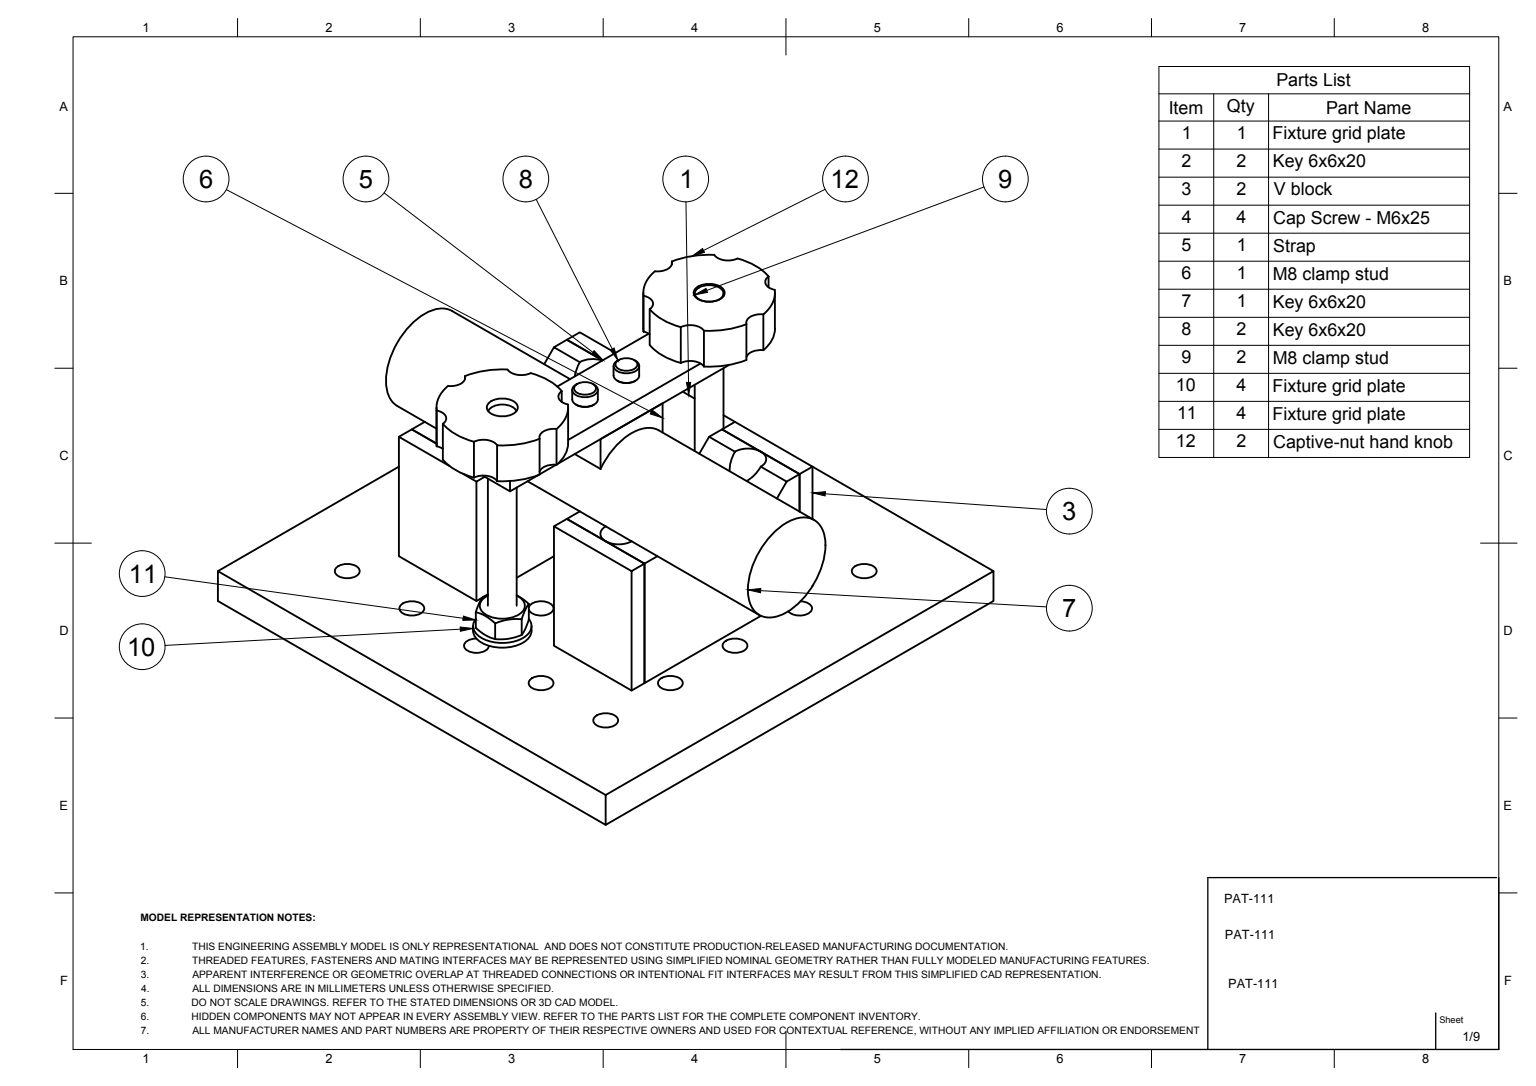
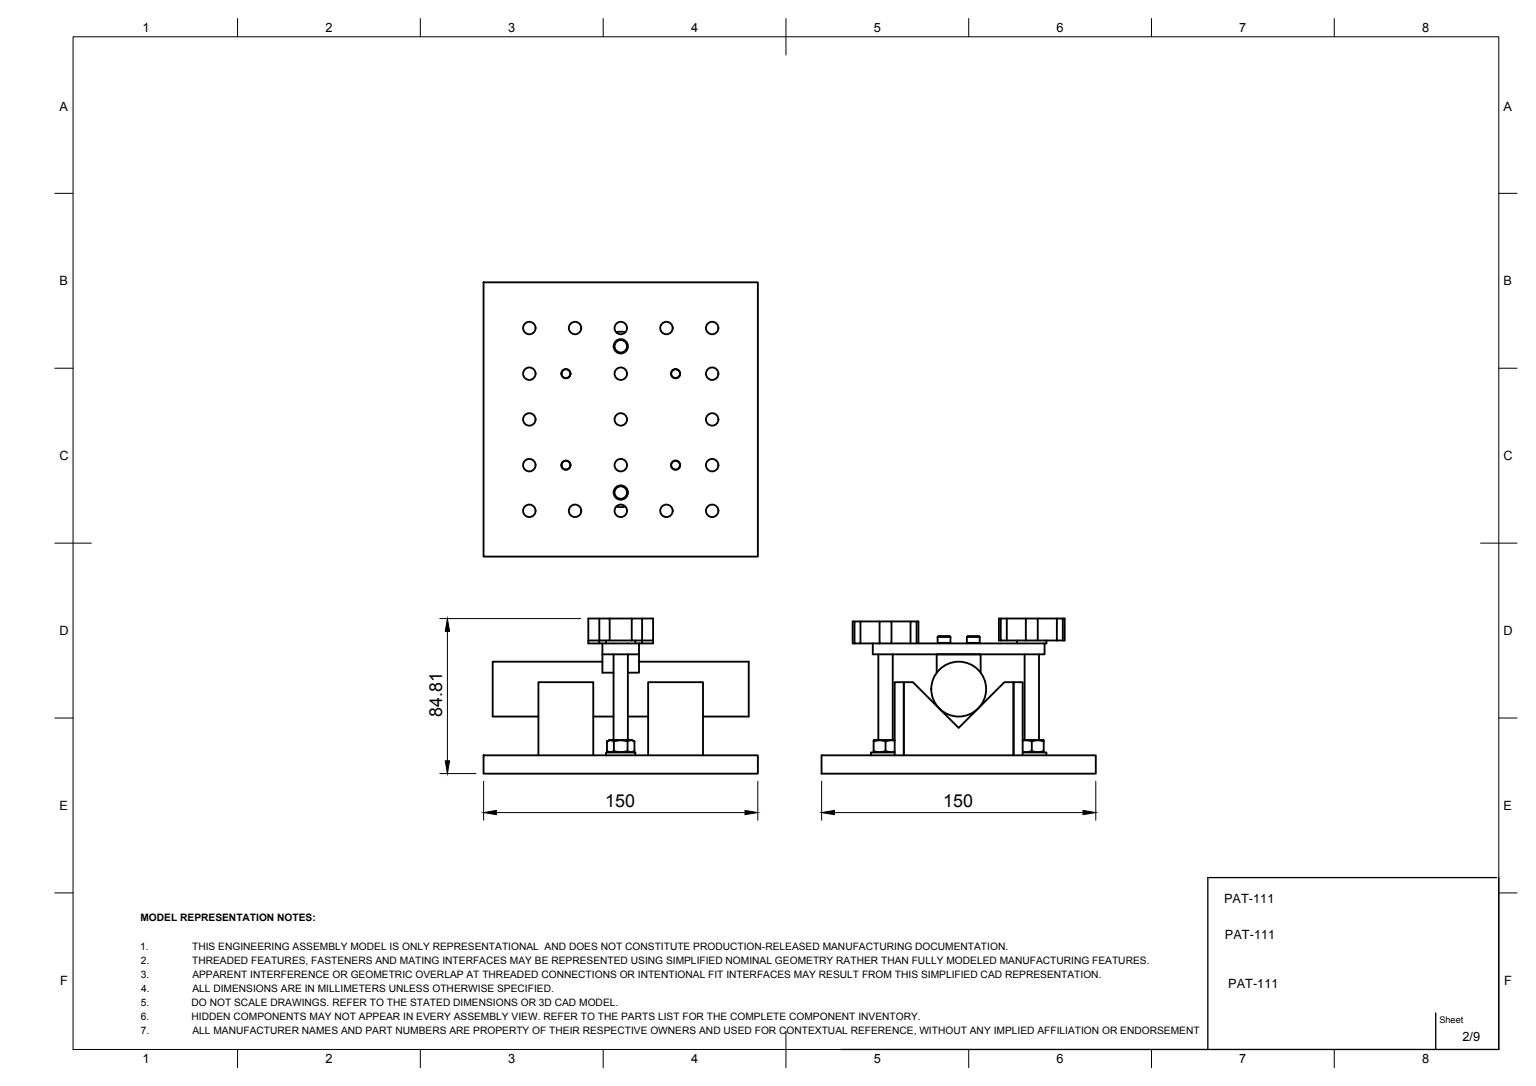
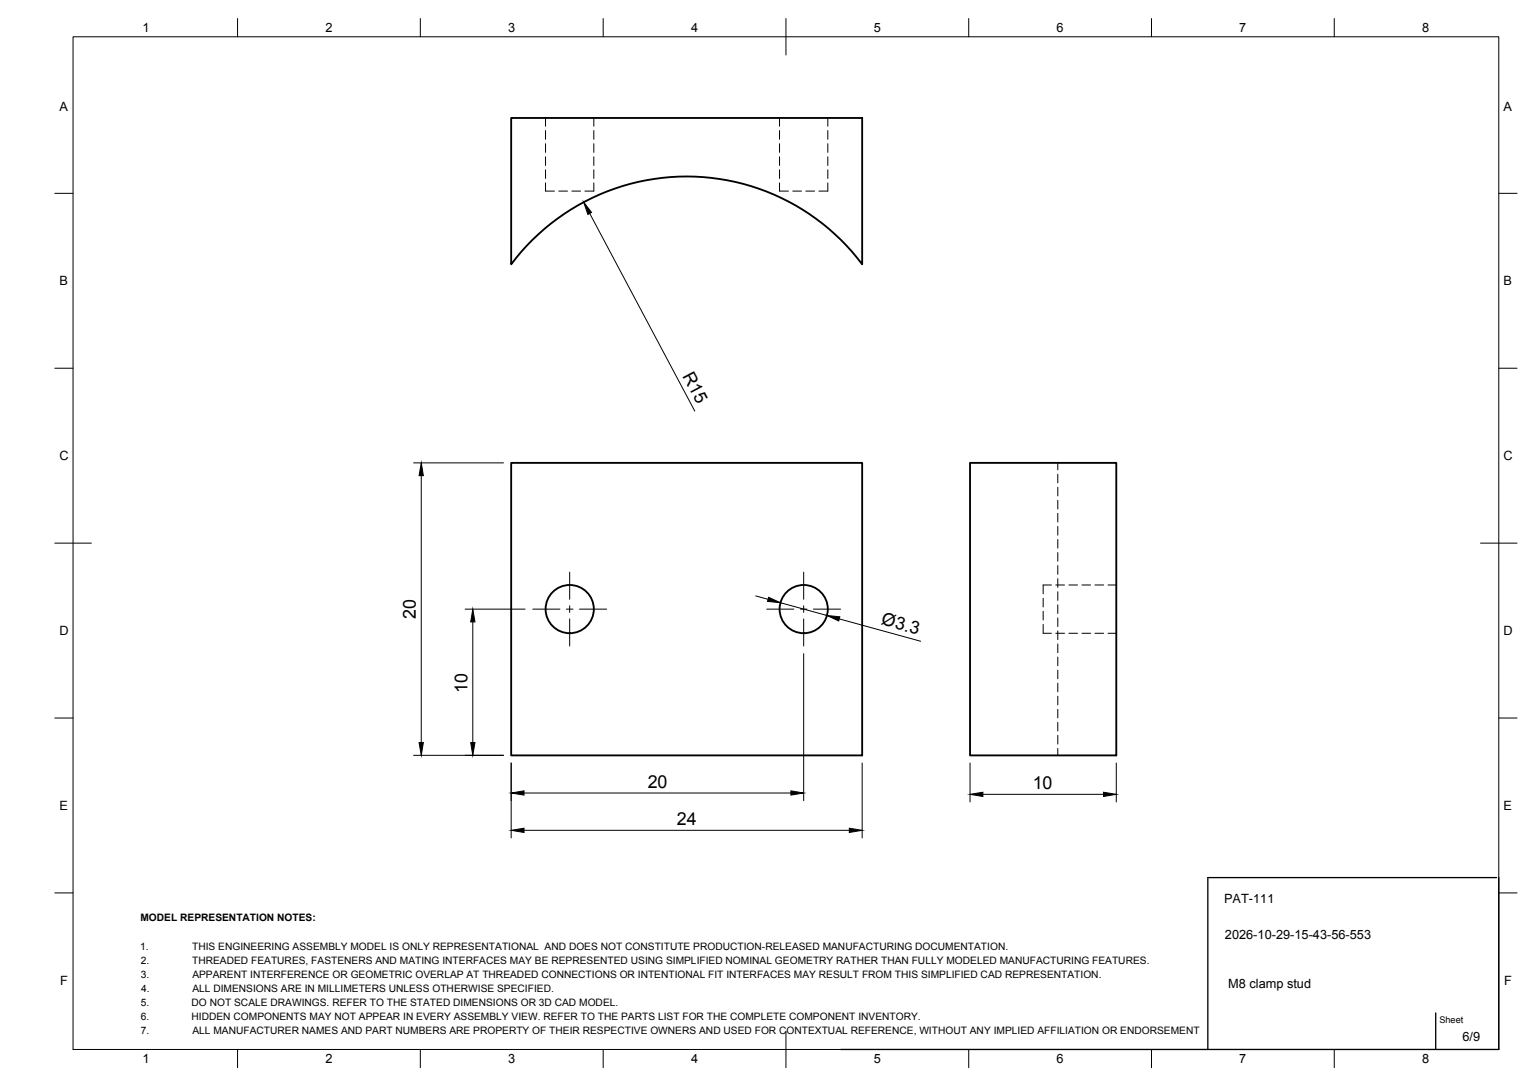
ISO-10303-21;
HEADER;
/* Generated by software containing ST-Developer
 * from STEP Tools, Inc. (www.steptools.com) 
 */

FILE_DESCRIPTION(
/* description */ ('Grid plate located blocks and clamp'),
/* implementation_level */ '2;1');

FILE_NAME(
/* name */ 'PAT-111',
/* time_stamp */ '2026-10-29T15:43:47-07:00',
/* author */ (''),
/* organization */ (''),
/* preprocessor_version */ 'ST-DEVELOPER v20.2',
/* originating_system */ 'Autodesk Translation Framework v15.17.0.0',
/* authorisation */ '');

FILE_SCHEMA (('AUTOMOTIVE_DESIGN { 1 0 10303 214 3 1 1 }'));
ENDSEC;

DATA;
#10=MECHANICAL_DESIGN_GEOMETRIC_PRESENTATION_REPRESENTATION('',(#166,#167,
#168,#169,#170,#171,#172,#173,#174,#175,#176,#177,#178,#179),#5702);
#11=ITEM_DEFINED_TRANSFORMATION($,$,#3411,#3737);
#12=ITEM_DEFINED_TRANSFORMATION($,$,#3688,#3738);
#13=ITEM_DEFINED_TRANSFORMATION($,$,#3503,#3739);
#14=ITEM_DEFINED_TRANSFORMATION($,$,#3514,#3740);
#15=ITEM_DEFINED_TRANSFORMATION($,$,#3565,#3741);
#16=ITEM_DEFINED_TRANSFORMATION($,$,#3565,#3742);
#17=ITEM_DEFINED_TRANSFORMATION($,$,#3503,#3743);
#18=ITEM_DEFINED_TRANSFORMATION($,$,#3514,#3744);
#19=ITEM_DEFINED_TRANSFORMATION($,$,#3565,#3745);
#20=ITEM_DEFINED_TRANSFORMATION($,$,#3565,#3746);
#21=ITEM_DEFINED_TRANSFORMATION($,$,#3591,#3747);
#22=ITEM_DEFINED_TRANSFORMATION($,$,#3610,#3748);
#23=ITEM_DEFINED_TRANSFORMATION($,$,#3627,#3749);
#24=ITEM_DEFINED_TRANSFORMATION($,$,#3633,#3750);
#25=ITEM_DEFINED_TRANSFORMATION($,$,#3633,#3751);
#26=ITEM_DEFINED_TRANSFORMATION($,$,#3657,#3752);
#27=ITEM_DEFINED_TRANSFORMATION($,$,#3663,#3753);
#28=ITEM_DEFINED_TRANSFORMATION($,$,#3663,#3754);
#29=ITEM_DEFINED_TRANSFORMATION($,$,#3672,#3755);
#30=ITEM_DEFINED_TRANSFORMATION($,$,#3672,#3756);
#31=ITEM_DEFINED_TRANSFORMATION($,$,#3657,#3757);
#32=ITEM_DEFINED_TRANSFORMATION($,$,#3663,#3758);
#33=ITEM_DEFINED_TRANSFORMATION($,$,#3663,#3759);
#34=ITEM_DEFINED_TRANSFORMATION($,$,#3672,#3760);
#35=ITEM_DEFINED_TRANSFORMATION($,$,#3672,#3761);
#36=ITEM_DEFINED_TRANSFORMATION($,$,#3688,#3762);
#37=(
REPRESENTATION_RELATIONSHIP($,$,#5760,#5759)
REPRESENTATION_RELATIONSHIP_WITH_TRANSFORMATION(#11)
SHAPE_REPRESENTATION_RELATIONSHIP()
);
#38=(
REPRESENTATION_RELATIONSHIP($,$,#5771,#5759)
REPRESENTATION_RELATIONSHIP_WITH_TRANSFORMATION(#12)
SHAPE_REPRESENTATION_RELATIONSHIP()
);
#39=(
REPRESENTATION_RELATIONSHIP($,$,#5761,#5759)
REPRESENTATION_RELATIONSHIP_WITH_TRANSFORMATION(#13)
SHAPE_REPRESENTATION_RELATIONSHIP()
);
#40=(
REPRESENTATION_RELATIONSHIP($,$,#5762,#5759)
REPRESENTATION_RELATIONSHIP_WITH_TRANSFORMATION(#14)
SHAPE_REPRESENTATION_RELATIONSHIP()
);
#41=(
REPRESENTATION_RELATIONSHIP($,$,#5763,#5759)
REPRESENTATION_RELATIONSHIP_WITH_TRANSFORMATION(#15)
SHAPE_REPRESENTATION_RELATIONSHIP()
);
#42=(
REPRESENTATION_RELATIONSHIP($,$,#5763,#5759)
REPRESENTATION_RELATIONSHIP_WITH_TRANSFORMATION(#16)
SHAPE_REPRESENTATION_RELATIONSHIP()
);
#43=(
REPRESENTATION_RELATIONSHIP($,$,#5761,#5759)
REPRESENTATION_RELATIONSHIP_WITH_TRANSFORMATION(#17)
SHAPE_REPRESENTATION_RELATIONSHIP()
);
#44=(
REPRESENTATION_RELATIONSHIP($,$,#5762,#5759)
REPRESENTATION_RELATIONSHIP_WITH_TRANSFORMATION(#18)
SHAPE_REPRESENTATION_RELATIONSHIP()
);
#45=(
REPRESENTATION_RELATIONSHIP($,$,#5763,#5759)
REPRESENTATION_RELATIONSHIP_WITH_TRANSFORMATION(#19)
SHAPE_REPRESENTATION_RELATIONSHIP()
);
#46=(
REPRESENTATION_RELATIONSHIP($,$,#5763,#5759)
REPRESENTATION_RELATIONSHIP_WITH_TRANSFORMATION(#20)
SHAPE_REPRESENTATION_RELATIONSHIP()
);
#47=(
REPRESENTATION_RELATIONSHIP($,$,#5764,#5759)
REPRESENTATION_RELATIONSHIP_WITH_TRANSFORMATION(#21)
SHAPE_REPRESENTATION_RELATIONSHIP()
);
#48=(
REPRESENTATION_RELATIONSHIP($,$,#5765,#5759)
REPRESENTATION_RELATIONSHIP_WITH_TRANSFORMATION(#22)
SHAPE_REPRESENTATION_RELATIONSHIP()
);
#49=(
REPRESENTATION_RELATIONSHIP($,$,#5766,#5759)
REPRESENTATION_RELATIONSHIP_WITH_TRANSFORMATION(#23)
SHAPE_REPRESENTATION_RELATIONSHIP()
);
#50=(
REPRESENTATION_RELATIONSHIP($,$,#5767,#5759)
REPRESENTATION_RELATIONSHIP_WITH_TRANSFORMATION(#24)
SHAPE_REPRESENTATION_RELATIONSHIP()
);
#51=(
REPRESENTATION_RELATIONSHIP($,$,#5767,#5759)
REPRESENTATION_RELATIONSHIP_WITH_TRANSFORMATION(#25)
SHAPE_REPRESENTATION_RELATIONSHIP()
);
#52=(
REPRESENTATION_RELATIONSHIP($,$,#5768,#5759)
REPRESENTATION_RELATIONSHIP_WITH_TRANSFORMATION(#26)
SHAPE_REPRESENTATION_RELATIONSHIP()
);
#53=(
REPRESENTATION_RELATIONSHIP($,$,#5769,#5759)
REPRESENTATION_RELATIONSHIP_WITH_TRANSFORMATION(#27)
SHAPE_REPRESENTATION_RELATIONSHIP()
);
#54=(
REPRESENTATION_RELATIONSHIP($,$,#5769,#5759)
REPRESENTATION_RELATIONSHIP_WITH_TRANSFORMATION(#28)
SHAPE_REPRESENTATION_RELATIONSHIP()
);
#55=(
REPRESENTATION_RELATIONSHIP($,$,#5770,#5759)
REPRESENTATION_RELATIONSHIP_WITH_TRANSFORMATION(#29)
SHAPE_REPRESENTATION_RELATIONSHIP()
);
#56=(
REPRESENTATION_RELATIONSHIP($,$,#5770,#5759)
REPRESENTATION_RELATIONSHIP_WITH_TRANSFORMATION(#30)
SHAPE_REPRESENTATION_RELATIONSHIP()
);
#57=(
REPRESENTATION_RELATIONSHIP($,$,#5768,#5759)
REPRESENTATION_RELATIONSHIP_WITH_TRANSFORMATION(#31)
SHAPE_REPRESENTATION_RELATIONSHIP()
);
#58=(
REPRESENTATION_RELATIONSHIP($,$,#5769,#5759)
REPRESENTATION_RELATIONSHIP_WITH_TRANSFORMATION(#32)
SHAPE_REPRESENTATION_RELATIONSHIP()
);
#59=(
REPRESENTATION_RELATIONSHIP($,$,#5769,#5759)
REPRESENTATION_RELATIONSHIP_WITH_TRANSFORMATION(#33)
SHAPE_REPRESENTATION_RELATIONSHIP()
);
#60=(
REPRESENTATION_RELATIONSHIP($,$,#5770,#5759)
REPRESENTATION_RELATIONSHIP_WITH_TRANSFORMATION(#34)
SHAPE_REPRESENTATION_RELATIONSHIP()
);
#61=(
REPRESENTATION_RELATIONSHIP($,$,#5770,#5759)
REPRESENTATION_RELATIONSHIP_WITH_TRANSFORMATION(#35)
SHAPE_REPRESENTATION_RELATIONSHIP()
);
#62=(
REPRESENTATION_RELATIONSHIP($,$,#5771,#5759)
REPRESENTATION_RELATIONSHIP_WITH_TRANSFORMATION(#36)
SHAPE_REPRESENTATION_RELATIONSHIP()
);
#63=CONTEXT_DEPENDENT_SHAPE_REPRESENTATION(#37,#5733);
#64=CONTEXT_DEPENDENT_SHAPE_REPRESENTATION(#38,#5734);
#65=CONTEXT_DEPENDENT_SHAPE_REPRESENTATION(#39,#5735);
#66=CONTEXT_DEPENDENT_SHAPE_REPRESENTATION(#40,#5736);
#67=CONTEXT_DEPENDENT_SHAPE_REPRESENTATION(#41,#5737);
#68=CONTEXT_DEPENDENT_SHAPE_REPRESENTATION(#42,#5738);
#69=CONTEXT_DEPENDENT_SHAPE_REPRESENTATION(#43,#5739);
#70=CONTEXT_DEPENDENT_SHAPE_REPRESENTATION(#44,#5740);
#71=CONTEXT_DEPENDENT_SHAPE_REPRESENTATION(#45,#5741);
#72=CONTEXT_DEPENDENT_SHAPE_REPRESENTATION(#46,#5742);
#73=CONTEXT_DEPENDENT_SHAPE_REPRESENTATION(#47,#5743);
#74=CONTEXT_DEPENDENT_SHAPE_REPRESENTATION(#48,#5744);
#75=CONTEXT_DEPENDENT_SHAPE_REPRESENTATION(#49,#5745);
#76=CONTEXT_DEPENDENT_SHAPE_REPRESENTATION(#50,#5746);
#77=CONTEXT_DEPENDENT_SHAPE_REPRESENTATION(#51,#5747);
#78=CONTEXT_DEPENDENT_SHAPE_REPRESENTATION(#52,#5748);
#79=CONTEXT_DEPENDENT_SHAPE_REPRESENTATION(#53,#5749);
#80=CONTEXT_DEPENDENT_SHAPE_REPRESENTATION(#54,#5750);
#81=CONTEXT_DEPENDENT_SHAPE_REPRESENTATION(#55,#5751);
#82=CONTEXT_DEPENDENT_SHAPE_REPRESENTATION(#56,#5752);
#83=CONTEXT_DEPENDENT_SHAPE_REPRESENTATION(#57,#5753);
#84=CONTEXT_DEPENDENT_SHAPE_REPRESENTATION(#58,#5754);
#85=CONTEXT_DEPENDENT_SHAPE_REPRESENTATION(#59,#5755);
#86=CONTEXT_DEPENDENT_SHAPE_REPRESENTATION(#60,#5756);
#87=CONTEXT_DEPENDENT_SHAPE_REPRESENTATION(#61,#5757);
#88=CONTEXT_DEPENDENT_SHAPE_REPRESENTATION(#62,#5758);
#89=NEXT_ASSEMBLY_USAGE_OCCURRENCE('Fixture grid plate:1',
'Fixture grid plate:1','Fixture grid plate:1',#5773,#5774,
'Fixture grid plate:1');
#90=NEXT_ASSEMBLY_USAGE_OCCURRENCE('Captive-nut hand knob:1',
'Captive-nut hand knob:1','Captive-nut hand knob:1',#5773,#5785,
'Captive-nut hand knob:1');
#91=NEXT_ASSEMBLY_USAGE_OCCURRENCE('Key 6x6x20:1','Key 6x6x20:1',
'Key 6x6x20:1',#5773,#5775,'Key 6x6x20:1');
#92=NEXT_ASSEMBLY_USAGE_OCCURRENCE('V block:1','V block:1','V block:1',
#5773,#5776,'V block:1');
#93=NEXT_ASSEMBLY_USAGE_OCCURRENCE('Cap Screw - M6x25:1',
'Cap Screw - M6x25:1','Cap Screw - M6x25:1',#5773,#5777,
'Cap Screw - M6x25:1');
#94=NEXT_ASSEMBLY_USAGE_OCCURRENCE('Cap Screw - M6x25:2',
'Cap Screw - M6x25:2','Cap Screw - M6x25:2',#5773,#5777,
'Cap Screw - M6x25:2');
#95=NEXT_ASSEMBLY_USAGE_OCCURRENCE('Key 6x6x20:2','Key 6x6x20:2',
'Key 6x6x20:2',#5773,#5775,'Key 6x6x20:2');
#96=NEXT_ASSEMBLY_USAGE_OCCURRENCE('V block:2','V block:2','V block:2',
#5773,#5776,'V block:2');
#97=NEXT_ASSEMBLY_USAGE_OCCURRENCE('Cap Screw - M6x25:3',
'Cap Screw - M6x25:3','Cap Screw - M6x25:3',#5773,#5777,
'Cap Screw - M6x25:3');
#98=NEXT_ASSEMBLY_USAGE_OCCURRENCE('Cap Screw - M6x25:4',
'Cap Screw - M6x25:4','Cap Screw - M6x25:4',#5773,#5777,
'Cap Screw - M6x25:4');
#99=NEXT_ASSEMBLY_USAGE_OCCURRENCE('Strap:1','Strap:1','Strap:1',#5773,
#5778,'Strap:1');
#100=NEXT_ASSEMBLY_USAGE_OCCURRENCE('Replaceable contact pad:1',
'Replaceable contact pad:1','Replaceable contact pad:1',#5773,#5779,
'Replaceable contact pad:1');
#101=NEXT_ASSEMBLY_USAGE_OCCURRENCE('Example round stock:1',
'Example round stock:1','Example round stock:1',#5773,#5780,
'Example round stock:1');
#102=NEXT_ASSEMBLY_USAGE_OCCURRENCE('M4x10 Cap Screw:1',
'M4x10 Cap Screw:1','M4x10 Cap Screw:1',#5773,#5781,'M4x10 Cap Screw:1');
#103=NEXT_ASSEMBLY_USAGE_OCCURRENCE('M4x10 Cap Screw:2',
'M4x10 Cap Screw:2','M4x10 Cap Screw:2',#5773,#5781,'M4x10 Cap Screw:2');
#104=NEXT_ASSEMBLY_USAGE_OCCURRENCE('M8 clamp stud:1','M8 clamp stud:1',
'M8 clamp stud:1',#5773,#5782,'M8 clamp stud:1');
#105=NEXT_ASSEMBLY_USAGE_OCCURRENCE('Flat Washer - M8:1',
'Flat Washer - M8:1','Flat Washer - M8:1',#5773,#5783,
'Flat Washer - M8:1');
#106=NEXT_ASSEMBLY_USAGE_OCCURRENCE('Flat Washer - M8:2',
'Flat Washer - M8:2','Flat Washer - M8:2',#5773,#5783,
'Flat Washer - M8:2');
#107=NEXT_ASSEMBLY_USAGE_OCCURRENCE('Hex Nut - M8:1','Hex Nut - M8:1',
'Hex Nut - M8:1',#5773,#5784,'Hex Nut - M8:1');
#108=NEXT_ASSEMBLY_USAGE_OCCURRENCE('Hex Nut - M8:2','Hex Nut - M8:2',
'Hex Nut - M8:2',#5773,#5784,'Hex Nut - M8:2');
#109=NEXT_ASSEMBLY_USAGE_OCCURRENCE('M8 clamp stud:2','M8 clamp stud:2',
'M8 clamp stud:2',#5773,#5782,'M8 clamp stud:2');
#110=NEXT_ASSEMBLY_USAGE_OCCURRENCE('Flat Washer - M8:3',
'Flat Washer - M8:3','Flat Washer - M8:3',#5773,#5783,
'Flat Washer - M8:3');
#111=NEXT_ASSEMBLY_USAGE_OCCURRENCE('Flat Washer - M8:4',
'Flat Washer - M8:4','Flat Washer - M8:4',#5773,#5783,
'Flat Washer - M8:4');
#112=NEXT_ASSEMBLY_USAGE_OCCURRENCE('Hex Nut - M8:3','Hex Nut - M8:3',
'Hex Nut - M8:3',#5773,#5784,'Hex Nut - M8:3');
#113=NEXT_ASSEMBLY_USAGE_OCCURRENCE('Hex Nut - M8:4','Hex Nut - M8:4',
'Hex Nut - M8:4',#5773,#5784,'Hex Nut - M8:4');
#114=NEXT_ASSEMBLY_USAGE_OCCURRENCE('Captive-nut hand knob:2',
'Captive-nut hand knob:2','Captive-nut hand knob:2',#5773,#5785,
'Captive-nut hand knob:2');
#115=(
BOUNDED_CURVE()
B_SPLINE_CURVE(2,(#5458,#5459,#5460),.UNSPECIFIED.,.F.,.F.)
B_SPLINE_CURVE_WITH_KNOTS((3,3),(0.14973948338295,0.97160236658079),
 .UNSPECIFIED.)
CURVE()
GEOMETRIC_REPRESENTATION_ITEM()
RATIONAL_B_SPLINE_CURVE((1.07140024848292,1.23714644374248,1.07140024848292))
REPRESENTATION_ITEM('')
);
#116=(
BOUNDED_CURVE()
B_SPLINE_CURVE(2,(#5462,#5463,#5464),.UNSPECIFIED.,.F.,.F.)
B_SPLINE_CURVE_WITH_KNOTS((3,3),(0.14973948338295,0.971602366580789),
 .UNSPECIFIED.)
CURVE()
GEOMETRIC_REPRESENTATION_ITEM()
RATIONAL_B_SPLINE_CURVE((1.07140024848292,1.23714644374248,1.07140024848292))
REPRESENTATION_ITEM('')
);
#117=(
BOUNDED_CURVE()
B_SPLINE_CURVE(2,(#5469,#5470,#5471),.UNSPECIFIED.,.F.,.F.)
B_SPLINE_CURVE_WITH_KNOTS((3,3),(0.14973948338295,0.97160236658079),
 .UNSPECIFIED.)
CURVE()
GEOMETRIC_REPRESENTATION_ITEM()
RATIONAL_B_SPLINE_CURVE((1.07140024848292,1.23714644374248,1.07140024848292))
REPRESENTATION_ITEM('')
);
#118=(
BOUNDED_CURVE()
B_SPLINE_CURVE(2,(#5473,#5474,#5475),.UNSPECIFIED.,.F.,.F.)
B_SPLINE_CURVE_WITH_KNOTS((3,3),(0.14973948338295,0.97160236658079),
 .UNSPECIFIED.)
CURVE()
GEOMETRIC_REPRESENTATION_ITEM()
RATIONAL_B_SPLINE_CURVE((1.07140024848292,1.23714644374248,1.07140024848292))
REPRESENTATION_ITEM('')
);
#119=(
BOUNDED_CURVE()
B_SPLINE_CURVE(2,(#5477,#5478,#5479),.UNSPECIFIED.,.F.,.F.)
B_SPLINE_CURVE_WITH_KNOTS((3,3),(0.14973948338295,0.971602366580789),
 .UNSPECIFIED.)
CURVE()
GEOMETRIC_REPRESENTATION_ITEM()
RATIONAL_B_SPLINE_CURVE((1.07140024848292,1.23714644374248,1.07140024848292))
REPRESENTATION_ITEM('')
);
#120=(
BOUNDED_CURVE()
B_SPLINE_CURVE(2,(#5480,#5481,#5482),.UNSPECIFIED.,.F.,.F.)
B_SPLINE_CURVE_WITH_KNOTS((3,3),(0.14973948338295,0.97160236658079),
 .UNSPECIFIED.)
CURVE()
GEOMETRIC_REPRESENTATION_ITEM()
RATIONAL_B_SPLINE_CURVE((1.07140024848292,1.23714644374248,1.07140024848292))
REPRESENTATION_ITEM('')
);
#121=(
BOUNDED_CURVE()
B_SPLINE_CURVE(2,(#5489,#5490,#5491),.UNSPECIFIED.,.F.,.F.)
B_SPLINE_CURVE_WITH_KNOTS((3,3),(0.14973948338295,0.97160236658079),
 .UNSPECIFIED.)
CURVE()
GEOMETRIC_REPRESENTATION_ITEM()
RATIONAL_B_SPLINE_CURVE((1.07140024848292,1.23714644374248,1.07140024848292))
REPRESENTATION_ITEM('')
);
#122=(
BOUNDED_CURVE()
B_SPLINE_CURVE(2,(#5493,#5494,#5495),.UNSPECIFIED.,.F.,.F.)
B_SPLINE_CURVE_WITH_KNOTS((3,3),(0.14973948338295,0.97160236658079),
 .UNSPECIFIED.)
CURVE()
GEOMETRIC_REPRESENTATION_ITEM()
RATIONAL_B_SPLINE_CURVE((1.07140024848292,1.23714644374248,1.07140024848292))
REPRESENTATION_ITEM('')
);
#123=(
BOUNDED_CURVE()
B_SPLINE_CURVE(2,(#5497,#5498,#5499),.UNSPECIFIED.,.F.,.F.)
B_SPLINE_CURVE_WITH_KNOTS((3,3),(0.14973948338295,0.971602366580789),
 .UNSPECIFIED.)
CURVE()
GEOMETRIC_REPRESENTATION_ITEM()
RATIONAL_B_SPLINE_CURVE((1.07140024848292,1.23714644374248,1.07140024848292))
REPRESENTATION_ITEM('')
);
#124=(
BOUNDED_CURVE()
B_SPLINE_CURVE(2,(#5501,#5502,#5503),.UNSPECIFIED.,.F.,.F.)
B_SPLINE_CURVE_WITH_KNOTS((3,3),(0.14973948338295,0.97160236658079),
 .UNSPECIFIED.)
CURVE()
GEOMETRIC_REPRESENTATION_ITEM()
RATIONAL_B_SPLINE_CURVE((1.07140024848292,1.23714644374248,1.07140024848292))
REPRESENTATION_ITEM('')
);
#125=(
BOUNDED_CURVE()
B_SPLINE_CURVE(2,(#5505,#5506,#5507),.UNSPECIFIED.,.F.,.F.)
B_SPLINE_CURVE_WITH_KNOTS((3,3),(0.14973948338295,0.97160236658079),
 .UNSPECIFIED.)
CURVE()
GEOMETRIC_REPRESENTATION_ITEM()
RATIONAL_B_SPLINE_CURVE((1.07140024848292,1.23714644374248,1.07140024848292))
REPRESENTATION_ITEM('')
);
#126=(
BOUNDED_CURVE()
B_SPLINE_CURVE(2,(#5508,#5509,#5510),.UNSPECIFIED.,.F.,.F.)
B_SPLINE_CURVE_WITH_KNOTS((3,3),(0.14973948338295,0.971602366580789),
 .UNSPECIFIED.)
CURVE()
GEOMETRIC_REPRESENTATION_ITEM()
RATIONAL_B_SPLINE_CURVE((1.07140024848292,1.23714644374248,1.07140024848292))
REPRESENTATION_ITEM('')
);
#127=ORIENTED_CLOSED_SHELL('',*,#3267,.F.);
#128=ORIENTED_CLOSED_SHELL('',*,#3271,.F.);
#129=CONICAL_SURFACE('',#3568,0.475,0.785398163397449);
#130=CONICAL_SURFACE('',#3572,0.485,0.785398163397448);
#131=CONICAL_SURFACE('',#3576,0.31,0.463647609000806);
#132=CONICAL_SURFACE('',#3580,0.27,0.785398163397448);
#133=CONICAL_SURFACE('',#3646,0.325,0.785398163397448);
#134=CONICAL_SURFACE('',#3650,0.335,0.785398163397448);
#135=CONICAL_SURFACE('',#3654,0.21,0.463647609000806);
#136=CONICAL_SURFACE('',#3673,0.734027674973257,1.0471975511966);
#137=CONICAL_SURFACE('',#3675,0.734027674973257,1.0471975511966);
#138=BREP_WITH_VOIDS('Body1',#3266,(#127));
#139=BREP_WITH_VOIDS('Body1',#3272,(#128));
#140=ELLIPSE('',#3521,0.707106781186547,0.5);
#141=ELLIPSE('',#3533,0.707106781186547,0.5);
#142=SHAPE_REPRESENTATION_RELATIONSHIP('SRR','None',#5760,#154);
#143=SHAPE_REPRESENTATION_RELATIONSHIP('SRR','None',#5761,#155);
#144=SHAPE_REPRESENTATION_RELATIONSHIP('SRR','None',#5762,#156);
#145=SHAPE_REPRESENTATION_RELATIONSHIP('SRR','None',#5763,#157);
#146=SHAPE_REPRESENTATION_RELATIONSHIP('SRR','None',#5764,#158);
#147=SHAPE_REPRESENTATION_RELATIONSHIP('SRR','None',#5765,#159);
#148=SHAPE_REPRESENTATION_RELATIONSHIP('SRR','None',#5766,#160);
#149=SHAPE_REPRESENTATION_RELATIONSHIP('SRR','None',#5767,#161);
#150=SHAPE_REPRESENTATION_RELATIONSHIP('SRR','None',#5768,#162);
#151=SHAPE_REPRESENTATION_RELATIONSHIP('SRR','None',#5769,#163);
#152=SHAPE_REPRESENTATION_RELATIONSHIP('SRR','None',#5770,#164);
#153=SHAPE_REPRESENTATION_RELATIONSHIP('SRR','None',#5771,#165);
#154=ADVANCED_BREP_SHAPE_REPRESENTATION('',(#180),#5690);
#155=ADVANCED_BREP_SHAPE_REPRESENTATION('',(#181),#5691);
#156=ADVANCED_BREP_SHAPE_REPRESENTATION('',(#182,#183,#184),#5692);
#157=ADVANCED_BREP_SHAPE_REPRESENTATION('',(#138),#5693);
#158=ADVANCED_BREP_SHAPE_REPRESENTATION('',(#185),#5694);
#159=ADVANCED_BREP_SHAPE_REPRESENTATION('',(#186),#5695);
#160=ADVANCED_BREP_SHAPE_REPRESENTATION('',(#187),#5696);
#161=ADVANCED_BREP_SHAPE_REPRESENTATION('',(#139),#5697);
#162=ADVANCED_BREP_SHAPE_REPRESENTATION('',(#188),#5698);
#163=ADVANCED_BREP_SHAPE_REPRESENTATION('',(#189),#5699);
#164=ADVANCED_BREP_SHAPE_REPRESENTATION('',(#190),#5700);
#165=ADVANCED_BREP_SHAPE_REPRESENTATION('',(#191),#5701);
#166=STYLED_ITEM('',(#5911),#180);
#167=STYLED_ITEM('',(#5897),#181);
#168=STYLED_ITEM('',(#5876),#182);
#169=STYLED_ITEM('',(#5876),#183);
#170=STYLED_ITEM('',(#5876),#184);
#171=STYLED_ITEM('',(#5904),#138);
#172=STYLED_ITEM('',(#5911),#185);
#173=STYLED_ITEM('',(#5890),#186);
#174=STYLED_ITEM('',(#5890),#187);
#175=STYLED_ITEM('',(#5904),#139);
#176=STYLED_ITEM('',(#5904),#188);
#177=STYLED_ITEM('',(#5904),#189);
#178=STYLED_ITEM('',(#5904),#190);
#179=STYLED_ITEM('',(#5904),#191);
#180=MANIFOLD_SOLID_BREP('Body1',#3261);
#181=MANIFOLD_SOLID_BREP('Body1',#3262);
#182=MANIFOLD_SOLID_BREP('Body1',#3263);
#183=MANIFOLD_SOLID_BREP('Body2',#3264);
#184=MANIFOLD_SOLID_BREP('Body3',#3265);
#185=MANIFOLD_SOLID_BREP('Body1',#3268);
#186=MANIFOLD_SOLID_BREP('Body1',#3269);
#187=MANIFOLD_SOLID_BREP('Body1',#3270);
#188=MANIFOLD_SOLID_BREP('Body1',#3273);
#189=MANIFOLD_SOLID_BREP('Body1',#3274);
#190=MANIFOLD_SOLID_BREP('Body1',#3275);
#191=MANIFOLD_SOLID_BREP('Body1',#3276);
#192=FACE_BOUND('',#680,.T.);
#193=FACE_BOUND('',#681,.T.);
#194=FACE_BOUND('',#682,.T.);
#195=FACE_BOUND('',#683,.T.);
#196=FACE_BOUND('',#684,.T.);
#197=FACE_BOUND('',#685,.T.);
#198=FACE_BOUND('',#686,.T.);
#199=FACE_BOUND('',#687,.T.);
#200=FACE_BOUND('',#688,.T.);
#201=FACE_BOUND('',#689,.T.);
#202=FACE_BOUND('',#690,.T.);
#203=FACE_BOUND('',#691,.T.);
#204=FACE_BOUND('',#692,.T.);
#205=FACE_BOUND('',#693,.T.);
#206=FACE_BOUND('',#694,.T.);
#207=FACE_BOUND('',#695,.T.);
#208=FACE_BOUND('',#696,.T.);
#209=FACE_BOUND('',#697,.T.);
#210=FACE_BOUND('',#698,.T.);
#211=FACE_BOUND('',#699,.T.);
#212=FACE_BOUND('',#700,.T.);
#213=FACE_BOUND('',#701,.T.);
#214=FACE_BOUND('',#702,.T.);
#215=FACE_BOUND('',#703,.T.);
#216=FACE_BOUND('',#704,.T.);
#217=FACE_BOUND('',#705,.T.);
#218=FACE_BOUND('',#706,.T.);
#219=FACE_BOUND('',#708,.T.);
#220=FACE_BOUND('',#709,.T.);
#221=FACE_BOUND('',#710,.T.);
#222=FACE_BOUND('',#711,.T.);
#223=FACE_BOUND('',#712,.T.);
#224=FACE_BOUND('',#713,.T.);
#225=FACE_BOUND('',#714,.T.);
#226=FACE_BOUND('',#715,.T.);
#227=FACE_BOUND('',#716,.T.);
#228=FACE_BOUND('',#717,.T.);
#229=FACE_BOUND('',#718,.T.);
#230=FACE_BOUND('',#719,.T.);
#231=FACE_BOUND('',#720,.T.);
#232=FACE_BOUND('',#721,.T.);
#233=FACE_BOUND('',#722,.T.);
#234=FACE_BOUND('',#723,.T.);
#235=FACE_BOUND('',#724,.T.);
#236=FACE_BOUND('',#725,.T.);
#237=FACE_BOUND('',#726,.T.);
#238=FACE_BOUND('',#727,.T.);
#239=FACE_BOUND('',#728,.T.);
#240=FACE_BOUND('',#729,.T.);
#241=FACE_BOUND('',#730,.T.);
#242=FACE_BOUND('',#731,.T.);
#243=FACE_BOUND('',#732,.T.);
#244=FACE_BOUND('',#752,.T.);
#245=FACE_BOUND('',#755,.T.);
#246=FACE_BOUND('',#769,.T.);
#247=FACE_BOUND('',#770,.T.);
#248=FACE_BOUND('',#771,.T.);
#249=FACE_BOUND('',#789,.T.);
#250=FACE_BOUND('',#811,.T.);
#251=FACE_BOUND('',#812,.T.);
#252=FACE_BOUND('',#813,.T.);
#253=FACE_BOUND('',#814,.T.);
#254=FACE_BOUND('',#816,.T.);
#255=FACE_BOUND('',#817,.T.);
#256=FACE_BOUND('',#818,.T.);
#257=FACE_BOUND('',#819,.T.);
#258=FACE_BOUND('',#830,.T.);
#259=FACE_BOUND('',#831,.T.);
#260=FACE_BOUND('',#849,.T.);
#261=FACE_BOUND('',#858,.T.);
#262=FACE_BOUND('',#860,.T.);
#263=FACE_BOUND('',#871,.T.);
#264=FACE_BOUND('',#873,.T.);
#265=FACE_BOUND('',#881,.T.);
#266=FACE_BOUND('',#895,.T.);
#267=FACE_BOUND('',#898,.T.);
#268=CIRCLE('',#3423,0.25);
#269=CIRCLE('',#3424,0.25);
#270=CIRCLE('',#3426,0.25);
#271=CIRCLE('',#3427,0.25);
#272=CIRCLE('',#3429,0.25);
#273=CIRCLE('',#3430,0.25);
#274=CIRCLE('',#3432,0.25);
#275=CIRCLE('',#3433,0.25);
#276=CIRCLE('',#3435,0.34);
#277=CIRCLE('',#3436,0.34);
#278=CIRCLE('',#3438,0.34);
#279=CIRCLE('',#3439,0.34);
#280=CIRCLE('',#3441,0.34);
#281=CIRCLE('',#3442,0.34);
#282=CIRCLE('',#3444,0.34);
#283=CIRCLE('',#3445,0.34);
#284=CIRCLE('',#3447,0.34);
#285=CIRCLE('',#3448,0.34);
#286=CIRCLE('',#3450,0.34);
#287=CIRCLE('',#3451,0.34);
#288=CIRCLE('',#3453,0.34);
#289=CIRCLE('',#3454,0.34);
#290=CIRCLE('',#3456,0.34);
#291=CIRCLE('',#3457,0.34);
#292=CIRCLE('',#3459,0.34);
#293=CIRCLE('',#3460,0.34);
#294=CIRCLE('',#3462,0.34);
#295=CIRCLE('',#3463,0.34);
#296=CIRCLE('',#3465,0.34);
#297=CIRCLE('',#3466,0.34);
#298=CIRCLE('',#3468,0.34);
#299=CIRCLE('',#3469,0.34);
#300=CIRCLE('',#3471,0.34);
#301=CIRCLE('',#3472,0.34);
#302=CIRCLE('',#3474,0.34);
#303=CIRCLE('',#3475,0.34);
#304=CIRCLE('',#3477,0.34);
#305=CIRCLE('',#3478,0.34);
#306=CIRCLE('',#3480,0.34);
#307=CIRCLE('',#3481,0.34);
#308=CIRCLE('',#3483,0.34);
#309=CIRCLE('',#3484,0.34);
#310=CIRCLE('',#3486,0.34);
#311=CIRCLE('',#3487,0.34);
#312=CIRCLE('',#3489,0.34);
#313=CIRCLE('',#3490,0.34);
#314=CIRCLE('',#3492,0.34);
#315=CIRCLE('',#3493,0.34);
#316=CIRCLE('',#3495,0.34);
#317=CIRCLE('',#3496,0.34);
#318=CIRCLE('',#3516,0.5);
#319=CIRCLE('',#3517,0.5);
#320=CIRCLE('',#3519,0.5);
#321=CIRCLE('',#3520,0.5);
#322=CIRCLE('',#3528,0.5);
#323=CIRCLE('',#3529,0.5);
#324=CIRCLE('',#3531,0.33);
#325=CIRCLE('',#3534,0.5);
#326=CIRCLE('',#3535,0.5);
#327=CIRCLE('',#3537,0.33);
#328=CIRCLE('',#3543,0.33);
#329=CIRCLE('',#3545,0.33);
#330=CIRCLE('',#3567,0.45);
#331=CIRCLE('',#3569,0.5);
#332=CIRCLE('',#3571,0.5);
#333=CIRCLE('',#3573,0.47);
#334=CIRCLE('',#3575,0.32);
#335=CIRCLE('',#3577,0.2942);
#336=CIRCLE('',#3579,0.2942);
#337=CIRCLE('',#3581,0.24);
#338=CIRCLE('',#3593,0.225);
#339=CIRCLE('',#3594,0.225);
#340=CIRCLE('',#3596,0.225);
#341=CIRCLE('',#3597,0.225);
#342=CIRCLE('',#3599,0.449999999999999);
#343=CIRCLE('',#3600,0.449999999999999);
#344=CIRCLE('',#3602,0.449999999999999);
#345=CIRCLE('',#3603,0.449999999999999);
#346=CIRCLE('',#3612,0.164999999999999);
#347=CIRCLE('',#3613,0.164999999999999);
#348=CIRCLE('',#3616,0.164999999999999);
#349=CIRCLE('',#3617,0.164999999999999);
#350=CIRCLE('',#3620,1.5);
#351=CIRCLE('',#3621,1.5);
#352=CIRCLE('',#3629,1.5);
#353=CIRCLE('',#3630,1.5);
#354=CIRCLE('',#3643,0.1954);
#355=CIRCLE('',#3645,0.3);
#356=CIRCLE('',#3647,0.35);
#357=CIRCLE('',#3649,0.35);
#358=CIRCLE('',#3651,0.32);
#359=CIRCLE('',#3653,0.22);
#360=CIRCLE('',#3655,0.1954);
#361=CIRCLE('',#3659,0.3933);
#362=CIRCLE('',#3660,0.3933);
#363=CIRCLE('',#3665,0.42);
#364=CIRCLE('',#3666,0.42);
#365=CIRCLE('',#3668,0.8);
#366=CIRCLE('',#3669,0.8);
#367=CIRCLE('',#3674,0.6175);
#368=CIRCLE('',#3676,0.6175);
#369=CIRCLE('',#3681,0.338975);
#370=CIRCLE('',#3682,0.338975);
#371=CIRCLE('',#3690,0.4);
#372=CIRCLE('',#3691,0.4);
#373=CIRCLE('',#3693,0.4);
#374=CIRCLE('',#3694,0.4);
#375=CIRCLE('',#3696,0.4);
#376=CIRCLE('',#3697,0.4);
#377=CIRCLE('',#3699,0.4);
#378=CIRCLE('',#3700,0.4);
#379=CIRCLE('',#3702,0.4);
#380=CIRCLE('',#3703,0.4);
#381=CIRCLE('',#3705,0.4);
#382=CIRCLE('',#3706,0.4);
#383=CIRCLE('',#3708,1.8);
#384=CIRCLE('',#3709,1.8);
#385=CIRCLE('',#3710,1.8);
#386=CIRCLE('',#3711,1.8);
#387=CIRCLE('',#3712,1.8);
#388=CIRCLE('',#3713,1.8);
#389=CIRCLE('',#3714,0.425);
#390=CIRCLE('',#3716,1.8);
#391=CIRCLE('',#3718,1.8);
#392=CIRCLE('',#3720,1.8);
#393=CIRCLE('',#3722,1.8);
#394=CIRCLE('',#3724,1.8);
#395=CIRCLE('',#3726,1.8);
#396=CIRCLE('',#3734,0.425);
#397=CYLINDRICAL_SURFACE('',#3422,0.25);
#398=CYLINDRICAL_SURFACE('',#3425,0.25);
#399=CYLINDRICAL_SURFACE('',#3428,0.25);
#400=CYLINDRICAL_SURFACE('',#3431,0.25);
#401=CYLINDRICAL_SURFACE('',#3434,0.34);
#402=CYLINDRICAL_SURFACE('',#3437,0.34);
#403=CYLINDRICAL_SURFACE('',#3440,0.34);
#404=CYLINDRICAL_SURFACE('',#3443,0.34);
#405=CYLINDRICAL_SURFACE('',#3446,0.34);
#406=CYLINDRICAL_SURFACE('',#3449,0.34);
#407=CYLINDRICAL_SURFACE('',#3452,0.34);
#408=CYLINDRICAL_SURFACE('',#3455,0.34);
#409=CYLINDRICAL_SURFACE('',#3458,0.34);
#410=CYLINDRICAL_SURFACE('',#3461,0.34);
#411=CYLINDRICAL_SURFACE('',#3464,0.34);
#412=CYLINDRICAL_SURFACE('',#3467,0.34);
#413=CYLINDRICAL_SURFACE('',#3470,0.34);
#414=CYLINDRICAL_SURFACE('',#3473,0.34);
#415=CYLINDRICAL_SURFACE('',#3476,0.34);
#416=CYLINDRICAL_SURFACE('',#3479,0.34);
#417=CYLINDRICAL_SURFACE('',#3482,0.34);
#418=CYLINDRICAL_SURFACE('',#3485,0.34);
#419=CYLINDRICAL_SURFACE('',#3488,0.34);
#420=CYLINDRICAL_SURFACE('',#3491,0.34);
#421=CYLINDRICAL_SURFACE('',#3494,0.34);
#422=CYLINDRICAL_SURFACE('',#3515,0.5);
#423=CYLINDRICAL_SURFACE('',#3518,0.5);
#424=CYLINDRICAL_SURFACE('',#3527,0.5);
#425=CYLINDRICAL_SURFACE('',#3532,0.5);
#426=CYLINDRICAL_SURFACE('',#3542,0.33);
#427=CYLINDRICAL_SURFACE('',#3544,0.33);
#428=CYLINDRICAL_SURFACE('',#3570,0.5);
#429=CYLINDRICAL_SURFACE('',#3578,0.2942);
#430=CYLINDRICAL_SURFACE('',#3592,0.225);
#431=CYLINDRICAL_SURFACE('',#3595,0.225);
#432=CYLINDRICAL_SURFACE('',#3598,0.449999999999999);
#433=CYLINDRICAL_SURFACE('',#3601,0.449999999999999);
#434=CYLINDRICAL_SURFACE('',#3611,0.164999999999999);
#435=CYLINDRICAL_SURFACE('',#3615,0.164999999999999);
#436=CYLINDRICAL_SURFACE('',#3619,1.5);
#437=CYLINDRICAL_SURFACE('',#3628,1.5);
#438=CYLINDRICAL_SURFACE('',#3648,0.35);
#439=CYLINDRICAL_SURFACE('',#3656,0.1954);
#440=CYLINDRICAL_SURFACE('',#3658,0.3933);
#441=CYLINDRICAL_SURFACE('',#3664,0.42);
#442=CYLINDRICAL_SURFACE('',#3667,0.8);
#443=CYLINDRICAL_SURFACE('',#3680,0.338975);
#444=CYLINDRICAL_SURFACE('',#3689,0.4);
#445=CYLINDRICAL_SURFACE('',#3692,0.4);
#446=CYLINDRICAL_SURFACE('',#3695,0.4);
#447=CYLINDRICAL_SURFACE('',#3698,0.4);
#448=CYLINDRICAL_SURFACE('',#3701,0.4);
#449=CYLINDRICAL_SURFACE('',#3704,0.4);
#450=CYLINDRICAL_SURFACE('',#3715,1.8);
#451=CYLINDRICAL_SURFACE('',#3717,1.8);
#452=CYLINDRICAL_SURFACE('',#3719,1.8);
#453=CYLINDRICAL_SURFACE('',#3721,1.8);
#454=CYLINDRICAL_SURFACE('',#3723,1.8);
#455=CYLINDRICAL_SURFACE('',#3725,1.8);
#456=CYLINDRICAL_SURFACE('',#3735,0.425);
#457=FACE_OUTER_BOUND('',#640,.T.);
#458=FACE_OUTER_BOUND('',#641,.T.);
#459=FACE_OUTER_BOUND('',#642,.T.);
#460=FACE_OUTER_BOUND('',#643,.T.);
#461=FACE_OUTER_BOUND('',#644,.T.);
#462=FACE_OUTER_BOUND('',#645,.T.);
#463=FACE_OUTER_BOUND('',#646,.T.);
#464=FACE_OUTER_BOUND('',#647,.T.);
#465=FACE_OUTER_BOUND('',#648,.T.);
#466=FACE_OUTER_BOUND('',#649,.T.);
#467=FACE_OUTER_BOUND('',#650,.T.);
#468=FACE_OUTER_BOUND('',#651,.T.);
#469=FACE_OUTER_BOUND('',#652,.T.);
#470=FACE_OUTER_BOUND('',#653,.T.);
#471=FACE_OUTER_BOUND('',#654,.T.);
#472=FACE_OUTER_BOUND('',#655,.T.);
#473=FACE_OUTER_BOUND('',#656,.T.);
#474=FACE_OUTER_BOUND('',#657,.T.);
#475=FACE_OUTER_BOUND('',#658,.T.);
#476=FACE_OUTER_BOUND('',#659,.T.);
#477=FACE_OUTER_BOUND('',#660,.T.);
#478=FACE_OUTER_BOUND('',#661,.T.);
#479=FACE_OUTER_BOUND('',#662,.T.);
#480=FACE_OUTER_BOUND('',#663,.T.);
#481=FACE_OUTER_BOUND('',#664,.T.);
#482=FACE_OUTER_BOUND('',#665,.T.);
#483=FACE_OUTER_BOUND('',#666,.T.);
#484=FACE_OUTER_BOUND('',#667,.T.);
#485=FACE_OUTER_BOUND('',#668,.T.);
#486=FACE_OUTER_BOUND('',#669,.T.);
#487=FACE_OUTER_BOUND('',#670,.T.);
#488=FACE_OUTER_BOUND('',#671,.T.);
#489=FACE_OUTER_BOUND('',#672,.T.);
#490=FACE_OUTER_BOUND('',#673,.T.);
#491=FACE_OUTER_BOUND('',#674,.T.);
#492=FACE_OUTER_BOUND('',#675,.T.);
#493=FACE_OUTER_BOUND('',#676,.T.);
#494=FACE_OUTER_BOUND('',#677,.T.);
#495=FACE_OUTER_BOUND('',#678,.T.);
#496=FACE_OUTER_BOUND('',#679,.T.);
#497=FACE_OUTER_BOUND('',#707,.T.);
#498=FACE_OUTER_BOUND('',#733,.T.);
#499=FACE_OUTER_BOUND('',#734,.T.);
#500=FACE_OUTER_BOUND('',#735,.T.);
#501=FACE_OUTER_BOUND('',#736,.T.);
#502=FACE_OUTER_BOUND('',#737,.T.);
#503=FACE_OUTER_BOUND('',#738,.T.);
#504=FACE_OUTER_BOUND('',#739,.T.);
#505=FACE_OUTER_BOUND('',#740,.T.);
#506=FACE_OUTER_BOUND('',#741,.T.);
#507=FACE_OUTER_BOUND('',#742,.T.);
#508=FACE_OUTER_BOUND('',#743,.T.);
#509=FACE_OUTER_BOUND('',#744,.T.);
#510=FACE_OUTER_BOUND('',#745,.T.);
#511=FACE_OUTER_BOUND('',#746,.T.);
#512=FACE_OUTER_BOUND('',#747,.T.);
#513=FACE_OUTER_BOUND('',#748,.T.);
#514=FACE_OUTER_BOUND('',#749,.T.);
#515=FACE_OUTER_BOUND('',#750,.T.);
#516=FACE_OUTER_BOUND('',#751,.T.);
#517=FACE_OUTER_BOUND('',#753,.T.);
#518=FACE_OUTER_BOUND('',#754,.T.);
#519=FACE_OUTER_BOUND('',#756,.T.);
#520=FACE_OUTER_BOUND('',#757,.T.);
#521=FACE_OUTER_BOUND('',#758,.T.);
#522=FACE_OUTER_BOUND('',#759,.T.);
#523=FACE_OUTER_BOUND('',#760,.T.);
#524=FACE_OUTER_BOUND('',#761,.T.);
#525=FACE_OUTER_BOUND('',#762,.T.);
#526=FACE_OUTER_BOUND('',#763,.T.);
#527=FACE_OUTER_BOUND('',#764,.T.);
#528=FACE_OUTER_BOUND('',#765,.T.);
#529=FACE_OUTER_BOUND('',#766,.T.);
#530=FACE_OUTER_BOUND('',#767,.T.);
#531=FACE_OUTER_BOUND('',#768,.T.);
#532=FACE_OUTER_BOUND('',#772,.T.);
#533=FACE_OUTER_BOUND('',#773,.T.);
#534=FACE_OUTER_BOUND('',#774,.T.);
#535=FACE_OUTER_BOUND('',#775,.T.);
#536=FACE_OUTER_BOUND('',#776,.T.);
#537=FACE_OUTER_BOUND('',#777,.T.);
#538=FACE_OUTER_BOUND('',#778,.T.);
#539=FACE_OUTER_BOUND('',#779,.T.);
#540=FACE_OUTER_BOUND('',#780,.T.);
#541=FACE_OUTER_BOUND('',#781,.T.);
#542=FACE_OUTER_BOUND('',#782,.T.);
#543=FACE_OUTER_BOUND('',#783,.T.);
#544=FACE_OUTER_BOUND('',#784,.T.);
#545=FACE_OUTER_BOUND('',#785,.T.);
#546=FACE_OUTER_BOUND('',#786,.T.);
#547=FACE_OUTER_BOUND('',#787,.T.);
#548=FACE_OUTER_BOUND('',#788,.T.);
#549=FACE_OUTER_BOUND('',#790,.T.);
#550=FACE_OUTER_BOUND('',#791,.T.);
#551=FACE_OUTER_BOUND('',#792,.T.);
#552=FACE_OUTER_BOUND('',#793,.T.);
#553=FACE_OUTER_BOUND('',#794,.T.);
#554=FACE_OUTER_BOUND('',#795,.T.);
#555=FACE_OUTER_BOUND('',#796,.T.);
#556=FACE_OUTER_BOUND('',#797,.T.);
#557=FACE_OUTER_BOUND('',#798,.T.);
#558=FACE_OUTER_BOUND('',#799,.T.);
#559=FACE_OUTER_BOUND('',#800,.T.);
#560=FACE_OUTER_BOUND('',#801,.T.);
#561=FACE_OUTER_BOUND('',#802,.T.);
#562=FACE_OUTER_BOUND('',#803,.T.);
#563=FACE_OUTER_BOUND('',#804,.T.);
#564=FACE_OUTER_BOUND('',#805,.T.);
#565=FACE_OUTER_BOUND('',#806,.T.);
#566=FACE_OUTER_BOUND('',#807,.T.);
#567=FACE_OUTER_BOUND('',#808,.T.);
#568=FACE_OUTER_BOUND('',#809,.T.);
#569=FACE_OUTER_BOUND('',#810,.T.);
#570=FACE_OUTER_BOUND('',#815,.T.);
#571=FACE_OUTER_BOUND('',#820,.T.);
#572=FACE_OUTER_BOUND('',#821,.T.);
#573=FACE_OUTER_BOUND('',#822,.T.);
#574=FACE_OUTER_BOUND('',#823,.T.);
#575=FACE_OUTER_BOUND('',#824,.T.);
#576=FACE_OUTER_BOUND('',#825,.T.);
#577=FACE_OUTER_BOUND('',#826,.T.);
#578=FACE_OUTER_BOUND('',#827,.T.);
#579=FACE_OUTER_BOUND('',#828,.T.);
#580=FACE_OUTER_BOUND('',#829,.T.);
#581=FACE_OUTER_BOUND('',#832,.T.);
#582=FACE_OUTER_BOUND('',#833,.T.);
#583=FACE_OUTER_BOUND('',#834,.T.);
#584=FACE_OUTER_BOUND('',#835,.T.);
#585=FACE_OUTER_BOUND('',#836,.T.);
#586=FACE_OUTER_BOUND('',#837,.T.);
#587=FACE_OUTER_BOUND('',#838,.T.);
#588=FACE_OUTER_BOUND('',#839,.T.);
#589=FACE_OUTER_BOUND('',#840,.T.);
#590=FACE_OUTER_BOUND('',#841,.T.);
#591=FACE_OUTER_BOUND('',#842,.T.);
#592=FACE_OUTER_BOUND('',#843,.T.);
#593=FACE_OUTER_BOUND('',#844,.T.);
#594=FACE_OUTER_BOUND('',#845,.T.);
#595=FACE_OUTER_BOUND('',#846,.T.);
#596=FACE_OUTER_BOUND('',#847,.T.);
#597=FACE_OUTER_BOUND('',#848,.T.);
#598=FACE_OUTER_BOUND('',#850,.T.);
#599=FACE_OUTER_BOUND('',#851,.T.);
#600=FACE_OUTER_BOUND('',#852,.T.);
#601=FACE_OUTER_BOUND('',#853,.T.);
#602=FACE_OUTER_BOUND('',#854,.T.);
#603=FACE_OUTER_BOUND('',#855,.T.);
#604=FACE_OUTER_BOUND('',#856,.T.);
#605=FACE_OUTER_BOUND('',#857,.T.);
#606=FACE_OUTER_BOUND('',#859,.T.);
#607=FACE_OUTER_BOUND('',#861,.T.);
#608=FACE_OUTER_BOUND('',#862,.T.);
#609=FACE_OUTER_BOUND('',#863,.T.);
#610=FACE_OUTER_BOUND('',#864,.T.);
#611=FACE_OUTER_BOUND('',#865,.T.);
#612=FACE_OUTER_BOUND('',#866,.T.);
#613=FACE_OUTER_BOUND('',#867,.T.);
#614=FACE_OUTER_BOUND('',#868,.T.);
#615=FACE_OUTER_BOUND('',#869,.T.);
#616=FACE_OUTER_BOUND('',#870,.T.);
#617=FACE_OUTER_BOUND('',#872,.T.);
#618=FACE_OUTER_BOUND('',#874,.T.);
#619=FACE_OUTER_BOUND('',#875,.T.);
#620=FACE_OUTER_BOUND('',#876,.T.);
#621=FACE_OUTER_BOUND('',#877,.T.);
#622=FACE_OUTER_BOUND('',#878,.T.);
#623=FACE_OUTER_BOUND('',#879,.T.);
#624=FACE_OUTER_BOUND('',#880,.T.);
#625=FACE_OUTER_BOUND('',#882,.T.);
#626=FACE_OUTER_BOUND('',#883,.T.);
#627=FACE_OUTER_BOUND('',#884,.T.);
#628=FACE_OUTER_BOUND('',#885,.T.);
#629=FACE_OUTER_BOUND('',#886,.T.);
#630=FACE_OUTER_BOUND('',#887,.T.);
#631=FACE_OUTER_BOUND('',#888,.T.);
#632=FACE_OUTER_BOUND('',#889,.T.);
#633=FACE_OUTER_BOUND('',#890,.T.);
#634=FACE_OUTER_BOUND('',#891,.T.);
#635=FACE_OUTER_BOUND('',#892,.T.);
#636=FACE_OUTER_BOUND('',#893,.T.);
#637=FACE_OUTER_BOUND('',#894,.T.);
#638=FACE_OUTER_BOUND('',#896,.T.);
#639=FACE_OUTER_BOUND('',#897,.T.);
#640=EDGE_LOOP('',(#2132,#2133,#2134,#2135));
#641=EDGE_LOOP('',(#2136,#2137,#2138,#2139));
#642=EDGE_LOOP('',(#2140,#2141,#2142,#2143));
#643=EDGE_LOOP('',(#2144,#2145,#2146,#2147));
#644=EDGE_LOOP('',(#2148,#2149,#2150,#2151));
#645=EDGE_LOOP('',(#2152,#2153,#2154,#2155));
#646=EDGE_LOOP('',(#2156,#2157,#2158,#2159));
#647=EDGE_LOOP('',(#2160,#2161,#2162,#2163));
#648=EDGE_LOOP('',(#2164,#2165,#2166,#2167));
#649=EDGE_LOOP('',(#2168,#2169,#2170,#2171));
#650=EDGE_LOOP('',(#2172,#2173,#2174,#2175));
#651=EDGE_LOOP('',(#2176,#2177,#2178,#2179));
#652=EDGE_LOOP('',(#2180,#2181,#2182,#2183));
#653=EDGE_LOOP('',(#2184,#2185,#2186,#2187));
#654=EDGE_LOOP('',(#2188,#2189,#2190,#2191));
#655=EDGE_LOOP('',(#2192,#2193,#2194,#2195));
#656=EDGE_LOOP('',(#2196,#2197,#2198,#2199));
#657=EDGE_LOOP('',(#2200,#2201,#2202,#2203));
#658=EDGE_LOOP('',(#2204,#2205,#2206,#2207));
#659=EDGE_LOOP('',(#2208,#2209,#2210,#2211));
#660=EDGE_LOOP('',(#2212,#2213,#2214,#2215));
#661=EDGE_LOOP('',(#2216,#2217,#2218,#2219));
#662=EDGE_LOOP('',(#2220,#2221,#2222,#2223));
#663=EDGE_LOOP('',(#2224,#2225,#2226,#2227));
#664=EDGE_LOOP('',(#2228,#2229,#2230,#2231));
#665=EDGE_LOOP('',(#2232,#2233,#2234,#2235));
#666=EDGE_LOOP('',(#2236,#2237,#2238,#2239));
#667=EDGE_LOOP('',(#2240,#2241,#2242,#2243));
#668=EDGE_LOOP('',(#2244,#2245,#2246,#2247));
#669=EDGE_LOOP('',(#2248,#2249,#2250,#2251));
#670=EDGE_LOOP('',(#2252,#2253,#2254,#2255));
#671=EDGE_LOOP('',(#2256,#2257,#2258,#2259));
#672=EDGE_LOOP('',(#2260,#2261,#2262,#2263));
#673=EDGE_LOOP('',(#2264,#2265,#2266,#2267));
#674=EDGE_LOOP('',(#2268,#2269,#2270,#2271));
#675=EDGE_LOOP('',(#2272,#2273,#2274,#2275));
#676=EDGE_LOOP('',(#2276,#2277,#2278,#2279));
#677=EDGE_LOOP('',(#2280,#2281,#2282,#2283));
#678=EDGE_LOOP('',(#2284,#2285,#2286,#2287));
#679=EDGE_LOOP('',(#2288,#2289,#2290,#2291));
#680=EDGE_LOOP('',(#2292,#2293,#2294,#2295));
#681=EDGE_LOOP('',(#2296));
#682=EDGE_LOOP('',(#2297));
#683=EDGE_LOOP('',(#2298));
#684=EDGE_LOOP('',(#2299));
#685=EDGE_LOOP('',(#2300));
#686=EDGE_LOOP('',(#2301));
#687=EDGE_LOOP('',(#2302));
#688=EDGE_LOOP('',(#2303));
#689=EDGE_LOOP('',(#2304));
#690=EDGE_LOOP('',(#2305));
#691=EDGE_LOOP('',(#2306));
#692=EDGE_LOOP('',(#2307));
#693=EDGE_LOOP('',(#2308));
#694=EDGE_LOOP('',(#2309));
#695=EDGE_LOOP('',(#2310));
#696=EDGE_LOOP('',(#2311));
#697=EDGE_LOOP('',(#2312));
#698=EDGE_LOOP('',(#2313));
#699=EDGE_LOOP('',(#2314));
#700=EDGE_LOOP('',(#2315));
#701=EDGE_LOOP('',(#2316));
#702=EDGE_LOOP('',(#2317));
#703=EDGE_LOOP('',(#2318));
#704=EDGE_LOOP('',(#2319));
#705=EDGE_LOOP('',(#2320));
#706=EDGE_LOOP('',(#2321,#2322,#2323,#2324));
#707=EDGE_LOOP('',(#2325,#2326,#2327,#2328));
#708=EDGE_LOOP('',(#2329));
#709=EDGE_LOOP('',(#2330));
#710=EDGE_LOOP('',(#2331));
#711=EDGE_LOOP('',(#2332));
#712=EDGE_LOOP('',(#2333));
#713=EDGE_LOOP('',(#2334));
#714=EDGE_LOOP('',(#2335));
#715=EDGE_LOOP('',(#2336));
#716=EDGE_LOOP('',(#2337));
#717=EDGE_LOOP('',(#2338));
#718=EDGE_LOOP('',(#2339));
#719=EDGE_LOOP('',(#2340));
#720=EDGE_LOOP('',(#2341));
#721=EDGE_LOOP('',(#2342));
#722=EDGE_LOOP('',(#2343));
#723=EDGE_LOOP('',(#2344));
#724=EDGE_LOOP('',(#2345));
#725=EDGE_LOOP('',(#2346));
#726=EDGE_LOOP('',(#2347));
#727=EDGE_LOOP('',(#2348));
#728=EDGE_LOOP('',(#2349));
#729=EDGE_LOOP('',(#2350));
#730=EDGE_LOOP('',(#2351));
#731=EDGE_LOOP('',(#2352));
#732=EDGE_LOOP('',(#2353));
#733=EDGE_LOOP('',(#2354,#2355,#2356,#2357,#2358,#2359,#2360,#2361));
#734=EDGE_LOOP('',(#2362,#2363,#2364,#2365));
#735=EDGE_LOOP('',(#2366,#2367,#2368,#2369));
#736=EDGE_LOOP('',(#2370,#2371,#2372,#2373));
#737=EDGE_LOOP('',(#2374,#2375,#2376,#2377));
#738=EDGE_LOOP('',(#2378,#2379,#2380,#2381,#2382,#2383,#2384,#2385));
#739=EDGE_LOOP('',(#2386,#2387,#2388,#2389));
#740=EDGE_LOOP('',(#2390,#2391,#2392,#2393));
#741=EDGE_LOOP('',(#2394,#2395,#2396,#2397));
#742=EDGE_LOOP('',(#2398,#2399,#2400,#2401));
#743=EDGE_LOOP('',(#2402,#2403,#2404,#2405));
#744=EDGE_LOOP('',(#2406,#2407,#2408,#2409,#2410));
#745=EDGE_LOOP('',(#2411,#2412,#2413,#2414));
#746=EDGE_LOOP('',(#2415,#2416,#2417,#2418));
#747=EDGE_LOOP('',(#2419,#2420,#2421,#2422));
#748=EDGE_LOOP('',(#2423,#2424,#2425,#2426));
#749=EDGE_LOOP('',(#2427,#2428,#2429,#2430));
#750=EDGE_LOOP('',(#2431,#2432,#2433,#2434));
#751=EDGE_LOOP('',(#2435,#2436));
#752=EDGE_LOOP('',(#2437));
#753=EDGE_LOOP('',(#2438,#2439,#2440,#2441,#2442));
#754=EDGE_LOOP('',(#2443,#2444));
#755=EDGE_LOOP('',(#2445));
#756=EDGE_LOOP('',(#2446,#2447,#2448,#2449,#2450,#2451));
#757=EDGE_LOOP('',(#2452,#2453,#2454,#2455));
#758=EDGE_LOOP('',(#2456,#2457,#2458,#2459,#2460,#2461));
#759=EDGE_LOOP('',(#2462,#2463,#2464,#2465));
#760=EDGE_LOOP('',(#2466,#2467,#2468,#2469));
#761=EDGE_LOOP('',(#2470,#2471,#2472,#2473));
#762=EDGE_LOOP('',(#2474,#2475,#2476,#2477));
#763=EDGE_LOOP('',(#2478,#2479,#2480,#2481));
#764=EDGE_LOOP('',(#2482,#2483,#2484,#2485,#2486,#2487,#2488));
#765=EDGE_LOOP('',(#2489,#2490,#2491,#2492,#2493,#2494,#2495));
#766=EDGE_LOOP('',(#2496,#2497,#2498,#2499,#2500,#2501,#2502));
#767=EDGE_LOOP('',(#2503,#2504,#2505,#2506,#2507,#2508,#2509));
#768=EDGE_LOOP('',(#2510,#2511,#2512,#2513));
#769=EDGE_LOOP('',(#2514,#2515,#2516,#2517));
#770=EDGE_LOOP('',(#2518));
#771=EDGE_LOOP('',(#2519));
#772=EDGE_LOOP('',(#2520,#2521,#2522,#2523));
#773=EDGE_LOOP('',(#2524,#2525,#2526,#2527));
#774=EDGE_LOOP('',(#2528,#2529,#2530,#2531));
#775=EDGE_LOOP('',(#2532,#2533,#2534,#2535));
#776=EDGE_LOOP('',(#2536,#2537,#2538,#2539));
#777=EDGE_LOOP('',(#2540,#2541,#2542,#2543));
#778=EDGE_LOOP('',(#2544,#2545,#2546,#2547));
#779=EDGE_LOOP('',(#2548,#2549,#2550,#2551));
#780=EDGE_LOOP('',(#2552,#2553,#2554,#2555));
#781=EDGE_LOOP('',(#2556,#2557,#2558,#2559));
#782=EDGE_LOOP('',(#2560,#2561,#2562,#2563));
#783=EDGE_LOOP('',(#2564,#2565,#2566,#2567));
#784=EDGE_LOOP('',(#2568));
#785=EDGE_LOOP('',(#2569,#2570,#2571,#2572));
#786=EDGE_LOOP('',(#2573,#2574,#2575,#2576));
#787=EDGE_LOOP('',(#2577,#2578,#2579,#2580));
#788=EDGE_LOOP('',(#2581));
#789=EDGE_LOOP('',(#2582));
#790=EDGE_LOOP('',(#2583,#2584,#2585,#2586));
#791=EDGE_LOOP('',(#2587,#2588,#2589,#2590));
#792=EDGE_LOOP('',(#2591,#2592,#2593,#2594));
#793=EDGE_LOOP('',(#2595));
#794=EDGE_LOOP('',(#2596,#2597,#2598,#2599));
#795=EDGE_LOOP('',(#2600,#2601,#2602,#2603));
#796=EDGE_LOOP('',(#2604,#2605,#2606,#2607));
#797=EDGE_LOOP('',(#2608,#2609,#2610,#2611));
#798=EDGE_LOOP('',(#2612,#2613,#2614,#2615));
#799=EDGE_LOOP('',(#2616,#2617,#2618,#2619));
#800=EDGE_LOOP('',(#2620,#2621,#2622,#2623,#2624,#2625));
#801=EDGE_LOOP('',(#2626,#2627,#2628,#2629,#2630,#2631));
#802=EDGE_LOOP('',(#2632,#2633,#2634,#2635));
#803=EDGE_LOOP('',(#2636,#2637,#2638,#2639));
#804=EDGE_LOOP('',(#2640,#2641,#2642,#2643));
#805=EDGE_LOOP('',(#2644,#2645,#2646,#2647));
#806=EDGE_LOOP('',(#2648,#2649,#2650,#2651));
#807=EDGE_LOOP('',(#2652,#2653,#2654,#2655));
#808=EDGE_LOOP('',(#2656,#2657,#2658,#2659));
#809=EDGE_LOOP('',(#2660,#2661,#2662,#2663));
#810=EDGE_LOOP('',(#2664,#2665,#2666,#2667));
#811=EDGE_LOOP('',(#2668));
#812=EDGE_LOOP('',(#2669));
#813=EDGE_LOOP('',(#2670));
#814=EDGE_LOOP('',(#2671));
#815=EDGE_LOOP('',(#2672,#2673,#2674,#2675));
#816=EDGE_LOOP('',(#2676));
#817=EDGE_LOOP('',(#2677));
#818=EDGE_LOOP('',(#2678));
#819=EDGE_LOOP('',(#2679));
#820=EDGE_LOOP('',(#2680,#2681,#2682,#2683));
#821=EDGE_LOOP('',(#2684));
#822=EDGE_LOOP('',(#2685,#2686,#2687,#2688));
#823=EDGE_LOOP('',(#2689));
#824=EDGE_LOOP('',(#2690,#2691,#2692,#2693));
#825=EDGE_LOOP('',(#2694,#2695,#2696,#2697));
#826=EDGE_LOOP('',(#2698,#2699,#2700,#2701));
#827=EDGE_LOOP('',(#2702,#2703,#2704,#2705));
#828=EDGE_LOOP('',(#2706,#2707,#2708,#2709));
#829=EDGE_LOOP('',(#2710,#2711,#2712,#2713));
#830=EDGE_LOOP('',(#2714));
#831=EDGE_LOOP('',(#2715));
#832=EDGE_LOOP('',(#2716,#2717,#2718,#2719));
#833=EDGE_LOOP('',(#2720));
#834=EDGE_LOOP('',(#2721));
#835=EDGE_LOOP('',(#2722,#2723,#2724,#2725));
#836=EDGE_LOOP('',(#2726,#2727,#2728,#2729));
#837=EDGE_LOOP('',(#2730,#2731,#2732,#2733));
#838=EDGE_LOOP('',(#2734,#2735,#2736,#2737));
#839=EDGE_LOOP('',(#2738,#2739,#2740,#2741));
#840=EDGE_LOOP('',(#2742,#2743,#2744,#2745));
#841=EDGE_LOOP('',(#2746,#2747,#2748,#2749,#2750,#2751));
#842=EDGE_LOOP('',(#2752,#2753,#2754,#2755,#2756,#2757));
#843=EDGE_LOOP('',(#2758));
#844=EDGE_LOOP('',(#2759));
#845=EDGE_LOOP('',(#2760,#2761,#2762,#2763));
#846=EDGE_LOOP('',(#2764,#2765,#2766,#2767));
#847=EDGE_LOOP('',(#2768,#2769,#2770,#2771));
#848=EDGE_LOOP('',(#2772));
#849=EDGE_LOOP('',(#2773));
#850=EDGE_LOOP('',(#2774,#2775,#2776,#2777));
#851=EDGE_LOOP('',(#2778,#2779,#2780,#2781));
#852=EDGE_LOOP('',(#2782,#2783,#2784,#2785));
#853=EDGE_LOOP('',(#2786));
#854=EDGE_LOOP('',(#2787));
#855=EDGE_LOOP('',(#2788,#2789,#2790,#2791));
#856=EDGE_LOOP('',(#2792,#2793,#2794,#2795));
#857=EDGE_LOOP('',(#2796));
#858=EDGE_LOOP('',(#2797));
#859=EDGE_LOOP('',(#2798));
#860=EDGE_LOOP('',(#2799));
#861=EDGE_LOOP('',(#2800,#2801,#2802,#2803,#2804,#2805,#2806,#2807,#2808));
#862=EDGE_LOOP('',(#2809,#2810,#2811,#2812,#2813,#2814,#2815,#2816,#2817));
#863=EDGE_LOOP('',(#2818,#2819,#2820,#2821));
#864=EDGE_LOOP('',(#2822,#2823,#2824,#2825));
#865=EDGE_LOOP('',(#2826,#2827,#2828,#2829));
#866=EDGE_LOOP('',(#2830,#2831,#2832,#2833));
#867=EDGE_LOOP('',(#2834,#2835,#2836,#2837));
#868=EDGE_LOOP('',(#2838,#2839,#2840,#2841));
#869=EDGE_LOOP('',(#2842,#2843,#2844,#2845));
#870=EDGE_LOOP('',(#2846));
#871=EDGE_LOOP('',(#2847));
#872=EDGE_LOOP('',(#2848));
#873=EDGE_LOOP('',(#2849));
#874=EDGE_LOOP('',(#2850,#2851,#2852,#2853));
#875=EDGE_LOOP('',(#2854,#2855,#2856,#2857));
#876=EDGE_LOOP('',(#2858,#2859,#2860,#2861));
#877=EDGE_LOOP('',(#2862,#2863,#2864,#2865));
#878=EDGE_LOOP('',(#2866,#2867,#2868,#2869));
#879=EDGE_LOOP('',(#2870,#2871,#2872,#2873));
#880=EDGE_LOOP('',(#2874,#2875,#2876,#2877,#2878,#2879,#2880,#2881,#2882,
#2883,#2884,#2885));
#881=EDGE_LOOP('',(#2886));
#882=EDGE_LOOP('',(#2887,#2888,#2889,#2890));
#883=EDGE_LOOP('',(#2891,#2892,#2893,#2894));
#884=EDGE_LOOP('',(#2895,#2896,#2897,#2898));
#885=EDGE_LOOP('',(#2899,#2900,#2901,#2902));
#886=EDGE_LOOP('',(#2903,#2904,#2905,#2906));
#887=EDGE_LOOP('',(#2907,#2908,#2909,#2910));
#888=EDGE_LOOP('',(#2911,#2912,#2913,#2914));
#889=EDGE_LOOP('',(#2915,#2916,#2917,#2918));
#890=EDGE_LOOP('',(#2919,#2920,#2921,#2922));
#891=EDGE_LOOP('',(#2923,#2924,#2925,#2926));
#892=EDGE_LOOP('',(#2927,#2928,#2929,#2930));
#893=EDGE_LOOP('',(#2931,#2932,#2933,#2934));
#894=EDGE_LOOP('',(#2935,#2936,#2937,#2938,#2939,#2940));
#895=EDGE_LOOP('',(#2941));
#896=EDGE_LOOP('',(#2942,#2943,#2944,#2945));
#897=EDGE_LOOP('',(#2946,#2947,#2948,#2949,#2950,#2951,#2952,#2953,#2954,
#2955,#2956,#2957));
#898=EDGE_LOOP('',(#2958,#2959,#2960,#2961,#2962,#2963));
#899=LINE('',#4747,#1172);
#900=LINE('',#4749,#1173);
#901=LINE('',#4751,#1174);
#902=LINE('',#4752,#1175);
#903=LINE('',#4755,#1176);
#904=LINE('',#4757,#1177);
#905=LINE('',#4758,#1178);
#906=LINE('',#4761,#1179);
#907=LINE('',#4763,#1180);
#908=LINE('',#4764,#1181);
#909=LINE('',#4766,#1182);
#910=LINE('',#4767,#1183);
#911=LINE('',#4772,#1184);
#912=LINE('',#4774,#1185);
#913=LINE('',#4776,#1186);
#914=LINE('',#4777,#1187);
#915=LINE('',#4780,#1188);
#916=LINE('',#4782,#1189);
#917=LINE('',#4783,#1190);
#918=LINE('',#4786,#1191);
#919=LINE('',#4788,#1192);
#920=LINE('',#4789,#1193);
#921=LINE('',#4791,#1194);
#922=LINE('',#4792,#1195);
#923=LINE('',#4798,#1196);
#924=LINE('',#4804,#1197);
#925=LINE('',#4810,#1198);
#926=LINE('',#4816,#1199);
#927=LINE('',#4822,#1200);
#928=LINE('',#4828,#1201);
#929=LINE('',#4834,#1202);
#930=LINE('',#4840,#1203);
#931=LINE('',#4846,#1204);
#932=LINE('',#4852,#1205);
#933=LINE('',#4858,#1206);
#934=LINE('',#4864,#1207);
#935=LINE('',#4870,#1208);
#936=LINE('',#4876,#1209);
#937=LINE('',#4882,#1210);
#938=LINE('',#4888,#1211);
#939=LINE('',#4894,#1212);
#940=LINE('',#4900,#1213);
#941=LINE('',#4906,#1214);
#942=LINE('',#4912,#1215);
#943=LINE('',#4918,#1216);
#944=LINE('',#4924,#1217);
#945=LINE('',#4930,#1218);
#946=LINE('',#4936,#1219);
#947=LINE('',#4942,#1220);
#948=LINE('',#4947,#1221);
#949=LINE('',#4949,#1222);
#950=LINE('',#4951,#1223);
#951=LINE('',#4952,#1224);
#952=LINE('',#4955,#1225);
#953=LINE('',#4957,#1226);
#954=LINE('',#4958,#1227);
#955=LINE('',#4961,#1228);
#956=LINE('',#4963,#1229);
#957=LINE('',#4964,#1230);
#958=LINE('',#4966,#1231);
#959=LINE('',#4967,#1232);
#960=LINE('',#4974,#1233);
#961=LINE('',#4976,#1234);
#962=LINE('',#4978,#1235);
#963=LINE('',#4980,#1236);
#964=LINE('',#4982,#1237);
#965=LINE('',#4984,#1238);
#966=LINE('',#4986,#1239);
#967=LINE('',#4987,#1240);
#968=LINE('',#4990,#1241);
#969=LINE('',#4992,#1242);
#970=LINE('',#4993,#1243);
#971=LINE('',#4996,#1244);
#972=LINE('',#4997,#1245);
#973=LINE('',#5000,#1246);
#974=LINE('',#5001,#1247);
#975=LINE('',#5004,#1248);
#976=LINE('',#5005,#1249);
#977=LINE('',#5009,#1250);
#978=LINE('',#5010,#1251);
#979=LINE('',#5012,#1252);
#980=LINE('',#5013,#1253);
#981=LINE('',#5015,#1254);
#982=LINE('',#5017,#1255);
#983=LINE('',#5019,#1256);
#984=LINE('',#5025,#1257);
#985=LINE('',#5029,#1258);
#986=LINE('',#5034,#1259);
#987=LINE('',#5038,#1260);
#988=LINE('',#5045,#1261);
#989=LINE('',#5047,#1262);
#990=LINE('',#5049,#1263);
#991=LINE('',#5050,#1264);
#992=LINE('',#5053,#1265);
#993=LINE('',#5055,#1266);
#994=LINE('',#5056,#1267);
#995=LINE('',#5059,#1268);
#996=LINE('',#5061,#1269);
#997=LINE('',#5062,#1270);
#998=LINE('',#5064,#1271);
#999=LINE('',#5065,#1272);
#1000=LINE('',#5069,#1273);
#1001=LINE('',#5078,#1274);
#1002=LINE('',#5085,#1275);
#1003=LINE('',#5087,#1276);
#1004=LINE('',#5089,#1277);
#1005=LINE('',#5091,#1278);
#1006=LINE('',#5092,#1279);
#1007=LINE('',#5095,#1280);
#1008=LINE('',#5096,#1281);
#1009=LINE('',#5099,#1282);
#1010=LINE('',#5100,#1283);
#1011=LINE('',#5102,#1284);
#1012=LINE('',#5103,#1285);
#1013=LINE('',#5106,#1286);
#1014=LINE('',#5107,#1287);
#1015=LINE('',#5111,#1288);
#1016=LINE('',#5115,#1289);
#1017=LINE('',#5118,#1290);
#1018=LINE('',#5119,#1291);
#1019=LINE('',#5122,#1292);
#1020=LINE('',#5123,#1293);
#1021=LINE('',#5126,#1294);
#1022=LINE('',#5128,#1295);
#1023=LINE('',#5129,#1296);
#1024=LINE('',#5132,#1297);
#1025=LINE('',#5133,#1298);
#1026=LINE('',#5136,#1299);
#1027=LINE('',#5137,#1300);
#1028=LINE('',#5139,#1301);
#1029=LINE('',#5144,#1302);
#1030=LINE('',#5146,#1303);
#1031=LINE('',#5148,#1304);
#1032=LINE('',#5149,#1305);
#1033=LINE('',#5152,#1306);
#1034=LINE('',#5154,#1307);
#1035=LINE('',#5155,#1308);
#1036=LINE('',#5158,#1309);
#1037=LINE('',#5160,#1310);
#1038=LINE('',#5161,#1311);
#1039=LINE('',#5163,#1312);
#1040=LINE('',#5164,#1313);
#1041=LINE('',#5170,#1314);
#1042=LINE('',#5172,#1315);
#1043=LINE('',#5174,#1316);
#1044=LINE('',#5175,#1317);
#1045=LINE('',#5178,#1318);
#1046=LINE('',#5180,#1319);
#1047=LINE('',#5181,#1320);
#1048=LINE('',#5184,#1321);
#1049=LINE('',#5186,#1322);
#1050=LINE('',#5187,#1323);
#1051=LINE('',#5189,#1324);
#1052=LINE('',#5190,#1325);
#1053=LINE('',#5200,#1326);
#1054=LINE('',#5204,#1327);
#1055=LINE('',#5208,#1328);
#1056=LINE('',#5215,#1329);
#1057=LINE('',#5219,#1330);
#1058=LINE('',#5223,#1331);
#1059=LINE('',#5228,#1332);
#1060=LINE('',#5230,#1333);
#1061=LINE('',#5232,#1334);
#1062=LINE('',#5233,#1335);
#1063=LINE('',#5236,#1336);
#1064=LINE('',#5238,#1337);
#1065=LINE('',#5239,#1338);
#1066=LINE('',#5242,#1339);
#1067=LINE('',#5244,#1340);
#1068=LINE('',#5245,#1341);
#1069=LINE('',#5248,#1342);
#1070=LINE('',#5250,#1343);
#1071=LINE('',#5251,#1344);
#1072=LINE('',#5254,#1345);
#1073=LINE('',#5256,#1346);
#1074=LINE('',#5257,#1347);
#1075=LINE('',#5259,#1348);
#1076=LINE('',#5260,#1349);
#1077=LINE('',#5268,#1350);
#1078=LINE('',#5274,#1351);
#1079=LINE('',#5280,#1352);
#1080=LINE('',#5286,#1353);
#1081=LINE('',#5291,#1354);
#1082=LINE('',#5293,#1355);
#1083=LINE('',#5295,#1356);
#1084=LINE('',#5296,#1357);
#1085=LINE('',#5299,#1358);
#1086=LINE('',#5301,#1359);
#1087=LINE('',#5302,#1360);
#1088=LINE('',#5305,#1361);
#1089=LINE('',#5307,#1362);
#1090=LINE('',#5308,#1363);
#1091=LINE('',#5310,#1364);
#1092=LINE('',#5311,#1365);
#1093=LINE('',#5319,#1366);
#1094=LINE('',#5326,#1367);
#1095=LINE('',#5332,#1368);
#1096=LINE('',#5336,#1369);
#1097=LINE('',#5340,#1370);
#1098=LINE('',#5342,#1371);
#1099=LINE('',#5343,#1372);
#1100=LINE('',#5346,#1373);
#1101=LINE('',#5347,#1374);
#1102=LINE('',#5350,#1375);
#1103=LINE('',#5351,#1376);
#1104=LINE('',#5353,#1377);
#1105=LINE('',#5360,#1378);
#1106=LINE('',#5368,#1379);
#1107=LINE('',#5370,#1380);
#1108=LINE('',#5372,#1381);
#1109=LINE('',#5373,#1382);
#1110=LINE('',#5376,#1383);
#1111=LINE('',#5378,#1384);
#1112=LINE('',#5379,#1385);
#1113=LINE('',#5382,#1386);
#1114=LINE('',#5384,#1387);
#1115=LINE('',#5385,#1388);
#1116=LINE('',#5388,#1389);
#1117=LINE('',#5390,#1390);
#1118=LINE('',#5391,#1391);
#1119=LINE('',#5394,#1392);
#1120=LINE('',#5396,#1393);
#1121=LINE('',#5397,#1394);
#1122=LINE('',#5399,#1395);
#1123=LINE('',#5400,#1396);
#1124=LINE('',#5412,#1397);
#1125=LINE('',#5416,#1398);
#1126=LINE('',#5420,#1399);
#1127=LINE('',#5427,#1400);
#1128=LINE('',#5429,#1401);
#1129=LINE('',#5435,#1402);
#1130=LINE('',#5444,#1403);
#1131=LINE('',#5450,#1404);
#1132=LINE('',#5466,#1405);
#1133=LINE('',#5487,#1406);
#1134=LINE('',#5512,#1407);
#1135=LINE('',#5513,#1408);
#1136=LINE('',#5515,#1409);
#1137=LINE('',#5517,#1410);
#1138=LINE('',#5522,#1411);
#1139=LINE('',#5525,#1412);
#1140=LINE('',#5527,#1413);
#1141=LINE('',#5535,#1414);
#1142=LINE('',#5539,#1415);
#1143=LINE('',#5544,#1416);
#1144=LINE('',#5548,#1417);
#1145=LINE('',#5553,#1418);
#1146=LINE('',#5557,#1419);
#1147=LINE('',#5562,#1420);
#1148=LINE('',#5566,#1421);
#1149=LINE('',#5571,#1422);
#1150=LINE('',#5575,#1423);
#1151=LINE('',#5580,#1424);
#1152=LINE('',#5584,#1425);
#1153=LINE('',#5610,#1426);
#1154=LINE('',#5612,#1427);
#1155=LINE('',#5614,#1428);
#1156=LINE('',#5615,#1429);
#1157=LINE('',#5618,#1430);
#1158=LINE('',#5620,#1431);
#1159=LINE('',#5621,#1432);
#1160=LINE('',#5624,#1433);
#1161=LINE('',#5626,#1434);
#1162=LINE('',#5627,#1435);
#1163=LINE('',#5630,#1436);
#1164=LINE('',#5632,#1437);
#1165=LINE('',#5633,#1438);
#1166=LINE('',#5636,#1439);
#1167=LINE('',#5638,#1440);
#1168=LINE('',#5639,#1441);
#1169=LINE('',#5641,#1442);
#1170=LINE('',#5642,#1443);
#1171=LINE('',#5647,#1444);
#1172=VECTOR('',#3769,1.);
#1173=VECTOR('',#3770,1.);
#1174=VECTOR('',#3771,1.);
#1175=VECTOR('',#3772,1.);
#1176=VECTOR('',#3775,1.);
#1177=VECTOR('',#3776,1.);
#1178=VECTOR('',#3777,1.);
#1179=VECTOR('',#3780,1.);
#1180=VECTOR('',#3781,1.);
#1181=VECTOR('',#3782,1.);
#1182=VECTOR('',#3785,1.);
#1183=VECTOR('',#3786,1.);
#1184=VECTOR('',#3791,1.);
#1185=VECTOR('',#3792,1.);
#1186=VECTOR('',#3793,1.);
#1187=VECTOR('',#3794,1.);
#1188=VECTOR('',#3797,1.);
#1189=VECTOR('',#3798,1.);
#1190=VECTOR('',#3799,1.);
#1191=VECTOR('',#3802,1.);
#1192=VECTOR('',#3803,1.);
#1193=VECTOR('',#3804,1.);
#1194=VECTOR('',#3807,1.);
#1195=VECTOR('',#3808,1.);
#1196=VECTOR('',#3815,0.25);
#1197=VECTOR('',#3822,0.25);
#1198=VECTOR('',#3829,0.25);
#1199=VECTOR('',#3836,0.25);
#1200=VECTOR('',#3843,0.34);
#1201=VECTOR('',#3850,0.34);
#1202=VECTOR('',#3857,0.34);
#1203=VECTOR('',#3864,0.34);
#1204=VECTOR('',#3871,0.34);
#1205=VECTOR('',#3878,0.34);
#1206=VECTOR('',#3885,0.34);
#1207=VECTOR('',#3892,0.34);
#1208=VECTOR('',#3899,0.34);
#1209=VECTOR('',#3906,0.34);
#1210=VECTOR('',#3913,0.34);
#1211=VECTOR('',#3920,0.34);
#1212=VECTOR('',#3927,0.34);
#1213=VECTOR('',#3934,0.34);
#1214=VECTOR('',#3941,0.34);
#1215=VECTOR('',#3948,0.34);
#1216=VECTOR('',#3955,0.34);
#1217=VECTOR('',#3962,0.34);
#1218=VECTOR('',#3969,0.34);
#1219=VECTOR('',#3976,0.34);
#1220=VECTOR('',#3983,0.34);
#1221=VECTOR('',#3988,1.);
#1222=VECTOR('',#3989,1.);
#1223=VECTOR('',#3990,1.);
#1224=VECTOR('',#3991,1.);
#1225=VECTOR('',#3994,1.);
#1226=VECTOR('',#3995,1.);
#1227=VECTOR('',#3996,1.);
#1228=VECTOR('',#3999,1.);
#1229=VECTOR('',#4000,1.);
#1230=VECTOR('',#4001,1.);
#1231=VECTOR('',#4004,1.);
#1232=VECTOR('',#4005,1.);
#1233=VECTOR('',#4014,1.);
#1234=VECTOR('',#4015,1.);
#1235=VECTOR('',#4016,1.);
#1236=VECTOR('',#4017,1.);
#1237=VECTOR('',#4018,1.);
#1238=VECTOR('',#4019,1.);
#1239=VECTOR('',#4020,1.);
#1240=VECTOR('',#4021,1.);
#1241=VECTOR('',#4024,1.);
#1242=VECTOR('',#4025,1.);
#1243=VECTOR('',#4026,1.);
#1244=VECTOR('',#4029,1.);
#1245=VECTOR('',#4030,1.);
#1246=VECTOR('',#4033,1.);
#1247=VECTOR('',#4034,1.);
#1248=VECTOR('',#4037,1.);
#1249=VECTOR('',#4038,1.);
#1250=VECTOR('',#4041,1.);
#1251=VECTOR('',#4042,1.);
#1252=VECTOR('',#4043,1.);
#1253=VECTOR('',#4044,1.);
#1254=VECTOR('',#4047,1.);
#1255=VECTOR('',#4050,1.);
#1256=VECTOR('',#4053,1.);
#1257=VECTOR('',#4060,0.5);
#1258=VECTOR('',#4063,1.);
#1259=VECTOR('',#4068,0.5);
#1260=VECTOR('',#4071,1.);
#1261=VECTOR('',#4078,1.);
#1262=VECTOR('',#4079,1.);
#1263=VECTOR('',#4080,1.);
#1264=VECTOR('',#4081,1.);
#1265=VECTOR('',#4084,1.);
#1266=VECTOR('',#4085,1.);
#1267=VECTOR('',#4086,1.);
#1268=VECTOR('',#4089,1.);
#1269=VECTOR('',#4090,1.);
#1270=VECTOR('',#4091,1.);
#1271=VECTOR('',#4094,1.);
#1272=VECTOR('',#4095,1.);
#1273=VECTOR('',#4102,1.);
#1274=VECTOR('',#4115,1.);
#1275=VECTOR('',#4124,1.);
#1276=VECTOR('',#4125,1.);
#1277=VECTOR('',#4126,1.);
#1278=VECTOR('',#4127,1.);
#1279=VECTOR('',#4128,1.);
#1280=VECTOR('',#4131,1.);
#1281=VECTOR('',#4132,1.);
#1282=VECTOR('',#4135,1.);
#1283=VECTOR('',#4136,1.);
#1284=VECTOR('',#4137,1.);
#1285=VECTOR('',#4138,1.);
#1286=VECTOR('',#4141,1.);
#1287=VECTOR('',#4142,1.);
#1288=VECTOR('',#4147,0.33);
#1289=VECTOR('',#4152,0.33);
#1290=VECTOR('',#4155,1.);
#1291=VECTOR('',#4156,1.);
#1292=VECTOR('',#4159,1.);
#1293=VECTOR('',#4160,1.);
#1294=VECTOR('',#4163,1.);
#1295=VECTOR('',#4164,1.);
#1296=VECTOR('',#4165,1.);
#1297=VECTOR('',#4168,1.);
#1298=VECTOR('',#4169,1.);
#1299=VECTOR('',#4172,1.);
#1300=VECTOR('',#4173,1.);
#1301=VECTOR('',#4176,1.);
#1302=VECTOR('',#4181,1.);
#1303=VECTOR('',#4182,1.);
#1304=VECTOR('',#4183,1.);
#1305=VECTOR('',#4184,1.);
#1306=VECTOR('',#4187,1.);
#1307=VECTOR('',#4188,1.);
#1308=VECTOR('',#4189,1.);
#1309=VECTOR('',#4192,1.);
#1310=VECTOR('',#4193,1.);
#1311=VECTOR('',#4194,1.);
#1312=VECTOR('',#4197,1.);
#1313=VECTOR('',#4198,1.);
#1314=VECTOR('',#4205,1.);
#1315=VECTOR('',#4206,1.);
#1316=VECTOR('',#4207,1.);
#1317=VECTOR('',#4208,1.);
#1318=VECTOR('',#4211,1.);
#1319=VECTOR('',#4212,1.);
#1320=VECTOR('',#4213,1.);
#1321=VECTOR('',#4216,1.);
#1322=VECTOR('',#4217,1.);
#1323=VECTOR('',#4218,1.);
#1324=VECTOR('',#4221,1.);
#1325=VECTOR('',#4222,1.);
#1326=VECTOR('',#4237,0.475);
#1327=VECTOR('',#4242,0.5);
#1328=VECTOR('',#4247,0.485);
#1329=VECTOR('',#4256,0.31);
#1330=VECTOR('',#4261,0.3);
#1331=VECTOR('',#4266,0.27);
#1332=VECTOR('',#4271,1.);
#1333=VECTOR('',#4272,1.);
#1334=VECTOR('',#4273,1.);
#1335=VECTOR('',#4274,1.);
#1336=VECTOR('',#4277,1.);
#1337=VECTOR('',#4278,1.);
#1338=VECTOR('',#4279,1.);
#1339=VECTOR('',#4282,1.);
#1340=VECTOR('',#4283,1.);
#1341=VECTOR('',#4284,1.);
#1342=VECTOR('',#4287,1.);
#1343=VECTOR('',#4288,1.);
#1344=VECTOR('',#4289,1.);
#1345=VECTOR('',#4292,1.);
#1346=VECTOR('',#4293,1.);
#1347=VECTOR('',#4294,1.);
#1348=VECTOR('',#4297,1.);
#1349=VECTOR('',#4298,1.);
#1350=VECTOR('',#4309,0.225);
#1351=VECTOR('',#4316,0.225);
#1352=VECTOR('',#4323,0.449999999999999);
#1353=VECTOR('',#4330,0.449999999999999);
#1354=VECTOR('',#4335,1.);
#1355=VECTOR('',#4336,1.);
#1356=VECTOR('',#4337,1.);
#1357=VECTOR('',#4338,1.);
#1358=VECTOR('',#4341,1.);
#1359=VECTOR('',#4342,1.);
#1360=VECTOR('',#4343,1.);
#1361=VECTOR('',#4346,1.);
#1362=VECTOR('',#4347,1.);
#1363=VECTOR('',#4348,1.);
#1364=VECTOR('',#4351,1.);
#1365=VECTOR('',#4352,1.);
#1366=VECTOR('',#4363,0.164999999999999);
#1367=VECTOR('',#4372,0.164999999999999);
#1368=VECTOR('',#4379,1.);
#1369=VECTOR('',#4382,1.);
#1370=VECTOR('',#4387,1.);
#1371=VECTOR('',#4388,1.);
#1372=VECTOR('',#4389,1.);
#1373=VECTOR('',#4392,1.);
#1374=VECTOR('',#4393,1.);
#1375=VECTOR('',#4396,1.);
#1376=VECTOR('',#4397,1.);
#1377=VECTOR('',#4400,1.);
#1378=VECTOR('',#4409,1.5);
#1379=VECTOR('',#4420,1.);
#1380=VECTOR('',#4421,1.);
#1381=VECTOR('',#4422,1.);
#1382=VECTOR('',#4423,1.);
#1383=VECTOR('',#4426,1.);
#1384=VECTOR('',#4427,1.);
#1385=VECTOR('',#4428,1.);
#1386=VECTOR('',#4431,1.);
#1387=VECTOR('',#4432,1.);
#1388=VECTOR('',#4433,1.);
#1389=VECTOR('',#4436,1.);
#1390=VECTOR('',#4437,1.);
#1391=VECTOR('',#4438,1.);
#1392=VECTOR('',#4441,1.);
#1393=VECTOR('',#4442,1.);
#1394=VECTOR('',#4443,1.);
#1395=VECTOR('',#4446,1.);
#1396=VECTOR('',#4447,1.);
#1397=VECTOR('',#4464,0.325);
#1398=VECTOR('',#4469,0.35);
#1399=VECTOR('',#4474,0.335);
#1400=VECTOR('',#4483,0.21);
#1401=VECTOR('',#4486,0.2);
#1402=VECTOR('',#4493,0.4);
#1403=VECTOR('',#4506,0.42);
#1404=VECTOR('',#4513,0.8);
#1405=VECTOR('',#4524,0.734027674973257);
#1406=VECTOR('',#4531,0.734027674973257);
#1407=VECTOR('',#4534,1.);
#1408=VECTOR('',#4535,1.);
#1409=VECTOR('',#4538,1.);
#1410=VECTOR('',#4541,1.);
#1411=VECTOR('',#4546,0.4);
#1412=VECTOR('',#4551,1.);
#1413=VECTOR('',#4554,1.);
#1414=VECTOR('',#4565,1.);
#1415=VECTOR('',#4568,1.);
#1416=VECTOR('',#4573,1.);
#1417=VECTOR('',#4576,1.);
#1418=VECTOR('',#4581,1.);
#1419=VECTOR('',#4584,1.);
#1420=VECTOR('',#4589,1.);
#1421=VECTOR('',#4592,1.);
#1422=VECTOR('',#4597,1.);
#1423=VECTOR('',#4600,1.);
#1424=VECTOR('',#4605,1.);
#1425=VECTOR('',#4608,1.);
#1426=VECTOR('',#4653,1.);
#1427=VECTOR('',#4654,1.);
#1428=VECTOR('',#4655,1.);
#1429=VECTOR('',#4656,1.);
#1430=VECTOR('',#4659,1.);
#1431=VECTOR('',#4660,1.);
#1432=VECTOR('',#4661,1.);
#1433=VECTOR('',#4664,1.);
#1434=VECTOR('',#4665,1.);
#1435=VECTOR('',#4666,1.);
#1436=VECTOR('',#4669,1.);
#1437=VECTOR('',#4670,1.);
#1438=VECTOR('',#4671,1.);
#1439=VECTOR('',#4674,1.);
#1440=VECTOR('',#4675,1.);
#1441=VECTOR('',#4676,1.);
#1442=VECTOR('',#4679,1.);
#1443=VECTOR('',#4680,1.);
#1444=VECTOR('',#4687,0.425);
#1445=VERTEX_POINT('',#4745);
#1446=VERTEX_POINT('',#4746);
#1447=VERTEX_POINT('',#4748);
#1448=VERTEX_POINT('',#4750);
#1449=VERTEX_POINT('',#4754);
#1450=VERTEX_POINT('',#4756);
#1451=VERTEX_POINT('',#4760);
#1452=VERTEX_POINT('',#4762);
#1453=VERTEX_POINT('',#4770);
#1454=VERTEX_POINT('',#4771);
#1455=VERTEX_POINT('',#4773);
#1456=VERTEX_POINT('',#4775);
#1457=VERTEX_POINT('',#4779);
#1458=VERTEX_POINT('',#4781);
#1459=VERTEX_POINT('',#4785);
#1460=VERTEX_POINT('',#4787);
#1461=VERTEX_POINT('',#4795);
#1462=VERTEX_POINT('',#4797);
#1463=VERTEX_POINT('',#4801);
#1464=VERTEX_POINT('',#4803);
#1465=VERTEX_POINT('',#4807);
#1466=VERTEX_POINT('',#4809);
#1467=VERTEX_POINT('',#4813);
#1468=VERTEX_POINT('',#4815);
#1469=VERTEX_POINT('',#4819);
#1470=VERTEX_POINT('',#4821);
#1471=VERTEX_POINT('',#4825);
#1472=VERTEX_POINT('',#4827);
#1473=VERTEX_POINT('',#4831);
#1474=VERTEX_POINT('',#4833);
#1475=VERTEX_POINT('',#4837);
#1476=VERTEX_POINT('',#4839);
#1477=VERTEX_POINT('',#4843);
#1478=VERTEX_POINT('',#4845);
#1479=VERTEX_POINT('',#4849);
#1480=VERTEX_POINT('',#4851);
#1481=VERTEX_POINT('',#4855);
#1482=VERTEX_POINT('',#4857);
#1483=VERTEX_POINT('',#4861);
#1484=VERTEX_POINT('',#4863);
#1485=VERTEX_POINT('',#4867);
#1486=VERTEX_POINT('',#4869);
#1487=VERTEX_POINT('',#4873);
#1488=VERTEX_POINT('',#4875);
#1489=VERTEX_POINT('',#4879);
#1490=VERTEX_POINT('',#4881);
#1491=VERTEX_POINT('',#4885);
#1492=VERTEX_POINT('',#4887);
#1493=VERTEX_POINT('',#4891);
#1494=VERTEX_POINT('',#4893);
#1495=VERTEX_POINT('',#4897);
#1496=VERTEX_POINT('',#4899);
#1497=VERTEX_POINT('',#4903);
#1498=VERTEX_POINT('',#4905);
#1499=VERTEX_POINT('',#4909);
#1500=VERTEX_POINT('',#4911);
#1501=VERTEX_POINT('',#4915);
#1502=VERTEX_POINT('',#4917);
#1503=VERTEX_POINT('',#4921);
#1504=VERTEX_POINT('',#4923);
#1505=VERTEX_POINT('',#4927);
#1506=VERTEX_POINT('',#4929);
#1507=VERTEX_POINT('',#4933);
#1508=VERTEX_POINT('',#4935);
#1509=VERTEX_POINT('',#4939);
#1510=VERTEX_POINT('',#4941);
#1511=VERTEX_POINT('',#4945);
#1512=VERTEX_POINT('',#4946);
#1513=VERTEX_POINT('',#4948);
#1514=VERTEX_POINT('',#4950);
#1515=VERTEX_POINT('',#4954);
#1516=VERTEX_POINT('',#4956);
#1517=VERTEX_POINT('',#4960);
#1518=VERTEX_POINT('',#4962);
#1519=VERTEX_POINT('',#4972);
#1520=VERTEX_POINT('',#4973);
#1521=VERTEX_POINT('',#4975);
#1522=VERTEX_POINT('',#4977);
#1523=VERTEX_POINT('',#4979);
#1524=VERTEX_POINT('',#4981);
#1525=VERTEX_POINT('',#4983);
#1526=VERTEX_POINT('',#4985);
#1527=VERTEX_POINT('',#4989);
#1528=VERTEX_POINT('',#4991);
#1529=VERTEX_POINT('',#4995);
#1530=VERTEX_POINT('',#4999);
#1531=VERTEX_POINT('',#5003);
#1532=VERTEX_POINT('',#5007);
#1533=VERTEX_POINT('',#5008);
#1534=VERTEX_POINT('',#5011);
#1535=VERTEX_POINT('',#5023);
#1536=VERTEX_POINT('',#5024);
#1537=VERTEX_POINT('',#5026);
#1538=VERTEX_POINT('',#5028);
#1539=VERTEX_POINT('',#5032);
#1540=VERTEX_POINT('',#5033);
#1541=VERTEX_POINT('',#5035);
#1542=VERTEX_POINT('',#5037);
#1543=VERTEX_POINT('',#5039);
#1544=VERTEX_POINT('',#5043);
#1545=VERTEX_POINT('',#5044);
#1546=VERTEX_POINT('',#5046);
#1547=VERTEX_POINT('',#5048);
#1548=VERTEX_POINT('',#5052);
#1549=VERTEX_POINT('',#5054);
#1550=VERTEX_POINT('',#5058);
#1551=VERTEX_POINT('',#5060);
#1552=VERTEX_POINT('',#5072);
#1553=VERTEX_POINT('',#5075);
#1554=VERTEX_POINT('',#5081);
#1555=VERTEX_POINT('',#5084);
#1556=VERTEX_POINT('',#5086);
#1557=VERTEX_POINT('',#5088);
#1558=VERTEX_POINT('',#5090);
#1559=VERTEX_POINT('',#5094);
#1560=VERTEX_POINT('',#5098);
#1561=VERTEX_POINT('',#5101);
#1562=VERTEX_POINT('',#5105);
#1563=VERTEX_POINT('',#5109);
#1564=VERTEX_POINT('',#5113);
#1565=VERTEX_POINT('',#5117);
#1566=VERTEX_POINT('',#5121);
#1567=VERTEX_POINT('',#5125);
#1568=VERTEX_POINT('',#5127);
#1569=VERTEX_POINT('',#5131);
#1570=VERTEX_POINT('',#5135);
#1571=VERTEX_POINT('',#5142);
#1572=VERTEX_POINT('',#5143);
#1573=VERTEX_POINT('',#5145);
#1574=VERTEX_POINT('',#5147);
#1575=VERTEX_POINT('',#5151);
#1576=VERTEX_POINT('',#5153);
#1577=VERTEX_POINT('',#5157);
#1578=VERTEX_POINT('',#5159);
#1579=VERTEX_POINT('',#5168);
#1580=VERTEX_POINT('',#5169);
#1581=VERTEX_POINT('',#5171);
#1582=VERTEX_POINT('',#5173);
#1583=VERTEX_POINT('',#5177);
#1584=VERTEX_POINT('',#5179);
#1585=VERTEX_POINT('',#5183);
#1586=VERTEX_POINT('',#5185);
#1587=VERTEX_POINT('',#5195);
#1588=VERTEX_POINT('',#5198);
#1589=VERTEX_POINT('',#5202);
#1590=VERTEX_POINT('',#5206);
#1591=VERTEX_POINT('',#5210);
#1592=VERTEX_POINT('',#5213);
#1593=VERTEX_POINT('',#5217);
#1594=VERTEX_POINT('',#5221);
#1595=VERTEX_POINT('',#5226);
#1596=VERTEX_POINT('',#5227);
#1597=VERTEX_POINT('',#5229);
#1598=VERTEX_POINT('',#5231);
#1599=VERTEX_POINT('',#5235);
#1600=VERTEX_POINT('',#5237);
#1601=VERTEX_POINT('',#5241);
#1602=VERTEX_POINT('',#5243);
#1603=VERTEX_POINT('',#5247);
#1604=VERTEX_POINT('',#5249);
#1605=VERTEX_POINT('',#5253);
#1606=VERTEX_POINT('',#5255);
#1607=VERTEX_POINT('',#5265);
#1608=VERTEX_POINT('',#5267);
#1609=VERTEX_POINT('',#5271);
#1610=VERTEX_POINT('',#5273);
#1611=VERTEX_POINT('',#5277);
#1612=VERTEX_POINT('',#5279);
#1613=VERTEX_POINT('',#5283);
#1614=VERTEX_POINT('',#5285);
#1615=VERTEX_POINT('',#5289);
#1616=VERTEX_POINT('',#5290);
#1617=VERTEX_POINT('',#5292);
#1618=VERTEX_POINT('',#5294);
#1619=VERTEX_POINT('',#5298);
#1620=VERTEX_POINT('',#5300);
#1621=VERTEX_POINT('',#5304);
#1622=VERTEX_POINT('',#5306);
#1623=VERTEX_POINT('',#5316);
#1624=VERTEX_POINT('',#5318);
#1625=VERTEX_POINT('',#5323);
#1626=VERTEX_POINT('',#5325);
#1627=VERTEX_POINT('',#5330);
#1628=VERTEX_POINT('',#5331);
#1629=VERTEX_POINT('',#5333);
#1630=VERTEX_POINT('',#5335);
#1631=VERTEX_POINT('',#5339);
#1632=VERTEX_POINT('',#5341);
#1633=VERTEX_POINT('',#5345);
#1634=VERTEX_POINT('',#5349);
#1635=VERTEX_POINT('',#5357);
#1636=VERTEX_POINT('',#5359);
#1637=VERTEX_POINT('',#5366);
#1638=VERTEX_POINT('',#5367);
#1639=VERTEX_POINT('',#5369);
#1640=VERTEX_POINT('',#5371);
#1641=VERTEX_POINT('',#5375);
#1642=VERTEX_POINT('',#5377);
#1643=VERTEX_POINT('',#5381);
#1644=VERTEX_POINT('',#5383);
#1645=VERTEX_POINT('',#5387);
#1646=VERTEX_POINT('',#5389);
#1647=VERTEX_POINT('',#5393);
#1648=VERTEX_POINT('',#5395);
#1649=VERTEX_POINT('',#5404);
#1650=VERTEX_POINT('',#5407);
#1651=VERTEX_POINT('',#5410);
#1652=VERTEX_POINT('',#5414);
#1653=VERTEX_POINT('',#5418);
#1654=VERTEX_POINT('',#5422);
#1655=VERTEX_POINT('',#5425);
#1656=VERTEX_POINT('',#5432);
#1657=VERTEX_POINT('',#5434);
#1658=VERTEX_POINT('',#5441);
#1659=VERTEX_POINT('',#5443);
#1660=VERTEX_POINT('',#5447);
#1661=VERTEX_POINT('',#5449);
#1662=VERTEX_POINT('',#5456);
#1663=VERTEX_POINT('',#5457);
#1664=VERTEX_POINT('',#5461);
#1665=VERTEX_POINT('',#5465);
#1666=VERTEX_POINT('',#5468);
#1667=VERTEX_POINT('',#5472);
#1668=VERTEX_POINT('',#5476);
#1669=VERTEX_POINT('',#5484);
#1670=VERTEX_POINT('',#5486);
#1671=VERTEX_POINT('',#5488);
#1672=VERTEX_POINT('',#5492);
#1673=VERTEX_POINT('',#5496);
#1674=VERTEX_POINT('',#5500);
#1675=VERTEX_POINT('',#5504);
#1676=VERTEX_POINT('',#5519);
#1677=VERTEX_POINT('',#5521);
#1678=VERTEX_POINT('',#5533);
#1679=VERTEX_POINT('',#5534);
#1680=VERTEX_POINT('',#5536);
#1681=VERTEX_POINT('',#5538);
#1682=VERTEX_POINT('',#5542);
#1683=VERTEX_POINT('',#5543);
#1684=VERTEX_POINT('',#5545);
#1685=VERTEX_POINT('',#5547);
#1686=VERTEX_POINT('',#5551);
#1687=VERTEX_POINT('',#5552);
#1688=VERTEX_POINT('',#5554);
#1689=VERTEX_POINT('',#5556);
#1690=VERTEX_POINT('',#5560);
#1691=VERTEX_POINT('',#5561);
#1692=VERTEX_POINT('',#5563);
#1693=VERTEX_POINT('',#5565);
#1694=VERTEX_POINT('',#5569);
#1695=VERTEX_POINT('',#5570);
#1696=VERTEX_POINT('',#5572);
#1697=VERTEX_POINT('',#5574);
#1698=VERTEX_POINT('',#5578);
#1699=VERTEX_POINT('',#5579);
#1700=VERTEX_POINT('',#5581);
#1701=VERTEX_POINT('',#5583);
#1702=VERTEX_POINT('',#5593);
#1703=VERTEX_POINT('',#5608);
#1704=VERTEX_POINT('',#5609);
#1705=VERTEX_POINT('',#5611);
#1706=VERTEX_POINT('',#5613);
#1707=VERTEX_POINT('',#5617);
#1708=VERTEX_POINT('',#5619);
#1709=VERTEX_POINT('',#5623);
#1710=VERTEX_POINT('',#5625);
#1711=VERTEX_POINT('',#5629);
#1712=VERTEX_POINT('',#5631);
#1713=VERTEX_POINT('',#5635);
#1714=VERTEX_POINT('',#5637);
#1715=VERTEX_POINT('',#5644);
#1716=EDGE_CURVE('',#1445,#1446,#899,.T.);
#1717=EDGE_CURVE('',#1447,#1445,#900,.T.);
#1718=EDGE_CURVE('',#1448,#1447,#901,.T.);
#1719=EDGE_CURVE('',#1448,#1446,#902,.T.);
#1720=EDGE_CURVE('',#1446,#1449,#903,.T.);
#1721=EDGE_CURVE('',#1450,#1448,#904,.T.);
#1722=EDGE_CURVE('',#1450,#1449,#905,.T.);
#1723=EDGE_CURVE('',#1449,#1451,#906,.T.);
#1724=EDGE_CURVE('',#1452,#1450,#907,.T.);
#1725=EDGE_CURVE('',#1452,#1451,#908,.T.);
#1726=EDGE_CURVE('',#1451,#1445,#909,.T.);
#1727=EDGE_CURVE('',#1447,#1452,#910,.T.);
#1728=EDGE_CURVE('',#1453,#1454,#911,.T.);
#1729=EDGE_CURVE('',#1455,#1453,#912,.T.);
#1730=EDGE_CURVE('',#1456,#1455,#913,.T.);
#1731=EDGE_CURVE('',#1456,#1454,#914,.T.);
#1732=EDGE_CURVE('',#1454,#1457,#915,.T.);
#1733=EDGE_CURVE('',#1458,#1456,#916,.T.);
#1734=EDGE_CURVE('',#1458,#1457,#917,.T.);
#1735=EDGE_CURVE('',#1457,#1459,#918,.T.);
#1736=EDGE_CURVE('',#1460,#1458,#919,.T.);
#1737=EDGE_CURVE('',#1460,#1459,#920,.T.);
#1738=EDGE_CURVE('',#1459,#1453,#921,.T.);
#1739=EDGE_CURVE('',#1455,#1460,#922,.T.);
#1740=EDGE_CURVE('',#1461,#1461,#268,.T.);
#1741=EDGE_CURVE('',#1461,#1462,#923,.T.);
#1742=EDGE_CURVE('',#1462,#1462,#269,.T.);
#1743=EDGE_CURVE('',#1463,#1463,#270,.T.);
#1744=EDGE_CURVE('',#1463,#1464,#924,.T.);
#1745=EDGE_CURVE('',#1464,#1464,#271,.T.);
#1746=EDGE_CURVE('',#1465,#1465,#272,.T.);
#1747=EDGE_CURVE('',#1465,#1466,#925,.T.);
#1748=EDGE_CURVE('',#1466,#1466,#273,.T.);
#1749=EDGE_CURVE('',#1467,#1467,#274,.T.);
#1750=EDGE_CURVE('',#1467,#1468,#926,.T.);
#1751=EDGE_CURVE('',#1468,#1468,#275,.T.);
#1752=EDGE_CURVE('',#1469,#1469,#276,.T.);
#1753=EDGE_CURVE('',#1469,#1470,#927,.T.);
#1754=EDGE_CURVE('',#1470,#1470,#277,.T.);
#1755=EDGE_CURVE('',#1471,#1471,#278,.T.);
#1756=EDGE_CURVE('',#1471,#1472,#928,.T.);
#1757=EDGE_CURVE('',#1472,#1472,#279,.T.);
#1758=EDGE_CURVE('',#1473,#1473,#280,.T.);
#1759=EDGE_CURVE('',#1473,#1474,#929,.T.);
#1760=EDGE_CURVE('',#1474,#1474,#281,.T.);
#1761=EDGE_CURVE('',#1475,#1475,#282,.T.);
#1762=EDGE_CURVE('',#1475,#1476,#930,.T.);
#1763=EDGE_CURVE('',#1476,#1476,#283,.T.);
#1764=EDGE_CURVE('',#1477,#1477,#284,.T.);
#1765=EDGE_CURVE('',#1477,#1478,#931,.T.);
#1766=EDGE_CURVE('',#1478,#1478,#285,.T.);
#1767=EDGE_CURVE('',#1479,#1479,#286,.T.);
#1768=EDGE_CURVE('',#1479,#1480,#932,.T.);
#1769=EDGE_CURVE('',#1480,#1480,#287,.T.);
#1770=EDGE_CURVE('',#1481,#1481,#288,.T.);
#1771=EDGE_CURVE('',#1481,#1482,#933,.T.);
#1772=EDGE_CURVE('',#1482,#1482,#289,.T.);
#1773=EDGE_CURVE('',#1483,#1483,#290,.T.);
#1774=EDGE_CURVE('',#1483,#1484,#934,.T.);
#1775=EDGE_CURVE('',#1484,#1484,#291,.T.);
#1776=EDGE_CURVE('',#1485,#1485,#292,.T.);
#1777=EDGE_CURVE('',#1485,#1486,#935,.T.);
#1778=EDGE_CURVE('',#1486,#1486,#293,.T.);
#1779=EDGE_CURVE('',#1487,#1487,#294,.T.);
#1780=EDGE_CURVE('',#1487,#1488,#936,.T.);
#1781=EDGE_CURVE('',#1488,#1488,#295,.T.);
#1782=EDGE_CURVE('',#1489,#1489,#296,.T.);
#1783=EDGE_CURVE('',#1489,#1490,#937,.T.);
#1784=EDGE_CURVE('',#1490,#1490,#297,.T.);
#1785=EDGE_CURVE('',#1491,#1491,#298,.T.);
#1786=EDGE_CURVE('',#1491,#1492,#938,.T.);
#1787=EDGE_CURVE('',#1492,#1492,#299,.T.);
#1788=EDGE_CURVE('',#1493,#1493,#300,.T.);
#1789=EDGE_CURVE('',#1493,#1494,#939,.T.);
#1790=EDGE_CURVE('',#1494,#1494,#301,.T.);
#1791=EDGE_CURVE('',#1495,#1495,#302,.T.);
#1792=EDGE_CURVE('',#1495,#1496,#940,.T.);
#1793=EDGE_CURVE('',#1496,#1496,#303,.T.);
#1794=EDGE_CURVE('',#1497,#1497,#304,.T.);
#1795=EDGE_CURVE('',#1497,#1498,#941,.T.);
#1796=EDGE_CURVE('',#1498,#1498,#305,.T.);
#1797=EDGE_CURVE('',#1499,#1499,#306,.T.);
#1798=EDGE_CURVE('',#1499,#1500,#942,.T.);
#1799=EDGE_CURVE('',#1500,#1500,#307,.T.);
#1800=EDGE_CURVE('',#1501,#1501,#308,.T.);
#1801=EDGE_CURVE('',#1501,#1502,#943,.T.);
#1802=EDGE_CURVE('',#1502,#1502,#309,.T.);
#1803=EDGE_CURVE('',#1503,#1503,#310,.T.);
#1804=EDGE_CURVE('',#1503,#1504,#944,.T.);
#1805=EDGE_CURVE('',#1504,#1504,#311,.T.);
#1806=EDGE_CURVE('',#1505,#1505,#312,.T.);
#1807=EDGE_CURVE('',#1505,#1506,#945,.T.);
#1808=EDGE_CURVE('',#1506,#1506,#313,.T.);
#1809=EDGE_CURVE('',#1507,#1507,#314,.T.);
#1810=EDGE_CURVE('',#1507,#1508,#946,.T.);
#1811=EDGE_CURVE('',#1508,#1508,#315,.T.);
#1812=EDGE_CURVE('',#1509,#1509,#316,.T.);
#1813=EDGE_CURVE('',#1509,#1510,#947,.T.);
#1814=EDGE_CURVE('',#1510,#1510,#317,.T.);
#1815=EDGE_CURVE('',#1511,#1512,#948,.T.);
#1816=EDGE_CURVE('',#1512,#1513,#949,.T.);
#1817=EDGE_CURVE('',#1514,#1513,#950,.T.);
#1818=EDGE_CURVE('',#1511,#1514,#951,.T.);
#1819=EDGE_CURVE('',#1515,#1511,#952,.T.);
#1820=EDGE_CURVE('',#1516,#1514,#953,.T.);
#1821=EDGE_CURVE('',#1515,#1516,#954,.T.);
#1822=EDGE_CURVE('',#1517,#1515,#955,.T.);
#1823=EDGE_CURVE('',#1518,#1516,#956,.T.);
#1824=EDGE_CURVE('',#1517,#1518,#957,.T.);
#1825=EDGE_CURVE('',#1512,#1517,#958,.T.);
#1826=EDGE_CURVE('',#1513,#1518,#959,.T.);
#1827=EDGE_CURVE('',#1519,#1520,#960,.T.);
#1828=EDGE_CURVE('',#1521,#1519,#961,.T.);
#1829=EDGE_CURVE('',#1522,#1521,#962,.T.);
#1830=EDGE_CURVE('',#1523,#1522,#963,.T.);
#1831=EDGE_CURVE('',#1524,#1523,#964,.T.);
#1832=EDGE_CURVE('',#1525,#1524,#965,.T.);
#1833=EDGE_CURVE('',#1526,#1525,#966,.T.);
#1834=EDGE_CURVE('',#1520,#1526,#967,.T.);
#1835=EDGE_CURVE('',#1523,#1527,#968,.T.);
#1836=EDGE_CURVE('',#1527,#1528,#969,.T.);
#1837=EDGE_CURVE('',#1528,#1524,#970,.T.);
#1838=EDGE_CURVE('',#1529,#1522,#971,.T.);
#1839=EDGE_CURVE('',#1529,#1527,#972,.T.);
#1840=EDGE_CURVE('',#1521,#1530,#973,.T.);
#1841=EDGE_CURVE('',#1530,#1529,#974,.T.);
#1842=EDGE_CURVE('',#1531,#1519,#975,.T.);
#1843=EDGE_CURVE('',#1531,#1530,#976,.T.);
#1844=EDGE_CURVE('',#1532,#1533,#977,.T.);
#1845=EDGE_CURVE('',#1528,#1532,#978,.T.);
#1846=EDGE_CURVE('',#1534,#1531,#979,.T.);
#1847=EDGE_CURVE('',#1533,#1534,#980,.T.);
#1848=EDGE_CURVE('',#1525,#1532,#981,.T.);
#1849=EDGE_CURVE('',#1520,#1534,#982,.T.);
#1850=EDGE_CURVE('',#1533,#1526,#983,.T.);
#1851=EDGE_CURVE('',#1535,#1536,#984,.T.);
#1852=EDGE_CURVE('',#1537,#1535,#318,.T.);
#1853=EDGE_CURVE('',#1537,#1538,#985,.T.);
#1854=EDGE_CURVE('',#1536,#1538,#319,.T.);
#1855=EDGE_CURVE('',#1539,#1540,#986,.T.);
#1856=EDGE_CURVE('',#1541,#1539,#320,.T.);
#1857=EDGE_CURVE('',#1541,#1542,#987,.T.);
#1858=EDGE_CURVE('',#1543,#1542,#321,.T.);
#1859=EDGE_CURVE('',#1540,#1543,#140,.T.);
#1860=EDGE_CURVE('',#1544,#1545,#988,.T.);
#1861=EDGE_CURVE('',#1544,#1546,#989,.T.);
#1862=EDGE_CURVE('',#1546,#1547,#990,.T.);
#1863=EDGE_CURVE('',#1545,#1547,#991,.T.);
#1864=EDGE_CURVE('',#1545,#1548,#992,.T.);
#1865=EDGE_CURVE('',#1547,#1549,#993,.T.);
#1866=EDGE_CURVE('',#1548,#1549,#994,.T.);
#1867=EDGE_CURVE('',#1548,#1550,#995,.T.);
#1868=EDGE_CURVE('',#1549,#1551,#996,.T.);
#1869=EDGE_CURVE('',#1550,#1551,#997,.T.);
#1870=EDGE_CURVE('',#1550,#1544,#998,.T.);
#1871=EDGE_CURVE('',#1551,#1546,#999,.T.);
#1872=EDGE_CURVE('',#1542,#1540,#322,.T.);
#1873=EDGE_CURVE('',#1541,#1542,#1000,.T.);
#1874=EDGE_CURVE('',#1539,#1541,#323,.T.);
#1875=EDGE_CURVE('',#1552,#1552,#324,.T.);
#1876=EDGE_CURVE('',#1553,#1536,#141,.T.);
#1877=EDGE_CURVE('',#1538,#1553,#325,.T.);
#1878=EDGE_CURVE('',#1537,#1538,#1001,.T.);
#1879=EDGE_CURVE('',#1535,#1537,#326,.T.);
#1880=EDGE_CURVE('',#1554,#1554,#327,.T.);
#1881=EDGE_CURVE('',#1555,#1543,#1002,.T.);
#1882=EDGE_CURVE('',#1556,#1555,#1003,.T.);
#1883=EDGE_CURVE('',#1557,#1556,#1004,.T.);
#1884=EDGE_CURVE('',#1558,#1557,#1005,.T.);
#1885=EDGE_CURVE('',#1540,#1558,#1006,.T.);
#1886=EDGE_CURVE('',#1542,#1559,#1007,.T.);
#1887=EDGE_CURVE('',#1559,#1555,#1008,.T.);
#1888=EDGE_CURVE('',#1560,#1536,#1009,.T.);
#1889=EDGE_CURVE('',#1557,#1560,#1010,.T.);
#1890=EDGE_CURVE('',#1561,#1556,#1011,.T.);
#1891=EDGE_CURVE('',#1553,#1561,#1012,.T.);
#1892=EDGE_CURVE('',#1538,#1562,#1013,.T.);
#1893=EDGE_CURVE('',#1562,#1560,#1014,.T.);
#1894=EDGE_CURVE('',#1563,#1563,#328,.T.);
#1895=EDGE_CURVE('',#1563,#1552,#1015,.T.);
#1896=EDGE_CURVE('',#1564,#1564,#329,.T.);
#1897=EDGE_CURVE('',#1564,#1554,#1016,.T.);
#1898=EDGE_CURVE('',#1558,#1565,#1017,.T.);
#1899=EDGE_CURVE('',#1565,#1542,#1018,.T.);
#1900=EDGE_CURVE('',#1561,#1566,#1019,.T.);
#1901=EDGE_CURVE('',#1566,#1538,#1020,.T.);
#1902=EDGE_CURVE('',#1567,#1562,#1021,.T.);
#1903=EDGE_CURVE('',#1567,#1568,#1022,.T.);
#1904=EDGE_CURVE('',#1568,#1565,#1023,.T.);
#1905=EDGE_CURVE('',#1569,#1567,#1024,.T.);
#1906=EDGE_CURVE('',#1569,#1566,#1025,.T.);
#1907=EDGE_CURVE('',#1570,#1559,#1026,.T.);
#1908=EDGE_CURVE('',#1570,#1569,#1027,.T.);
#1909=EDGE_CURVE('',#1568,#1570,#1028,.T.);
#1910=EDGE_CURVE('',#1571,#1572,#1029,.T.);
#1911=EDGE_CURVE('',#1572,#1573,#1030,.T.);
#1912=EDGE_CURVE('',#1574,#1573,#1031,.T.);
#1913=EDGE_CURVE('',#1571,#1574,#1032,.T.);
#1914=EDGE_CURVE('',#1575,#1571,#1033,.T.);
#1915=EDGE_CURVE('',#1576,#1574,#1034,.T.);
#1916=EDGE_CURVE('',#1575,#1576,#1035,.T.);
#1917=EDGE_CURVE('',#1577,#1575,#1036,.T.);
#1918=EDGE_CURVE('',#1578,#1576,#1037,.T.);
#1919=EDGE_CURVE('',#1577,#1578,#1038,.T.);
#1920=EDGE_CURVE('',#1572,#1577,#1039,.T.);
#1921=EDGE_CURVE('',#1573,#1578,#1040,.T.);
#1922=EDGE_CURVE('',#1579,#1580,#1041,.T.);
#1923=EDGE_CURVE('',#1580,#1581,#1042,.T.);
#1924=EDGE_CURVE('',#1582,#1581,#1043,.T.);
#1925=EDGE_CURVE('',#1579,#1582,#1044,.T.);
#1926=EDGE_CURVE('',#1583,#1579,#1045,.T.);
#1927=EDGE_CURVE('',#1584,#1582,#1046,.T.);
#1928=EDGE_CURVE('',#1583,#1584,#1047,.T.);
#1929=EDGE_CURVE('',#1585,#1583,#1048,.T.);
#1930=EDGE_CURVE('',#1586,#1584,#1049,.T.);
#1931=EDGE_CURVE('',#1585,#1586,#1050,.T.);
#1932=EDGE_CURVE('',#1580,#1585,#1051,.T.);
#1933=EDGE_CURVE('',#1581,#1586,#1052,.T.);
#1934=EDGE_CURVE('',#1587,#1587,#330,.T.);
#1935=EDGE_CURVE('',#1588,#1588,#331,.T.);
#1936=EDGE_CURVE('',#1588,#1587,#1053,.T.);
#1937=EDGE_CURVE('',#1589,#1589,#332,.T.);
#1938=EDGE_CURVE('',#1589,#1588,#1054,.T.);
#1939=EDGE_CURVE('',#1590,#1590,#333,.T.);
#1940=EDGE_CURVE('',#1590,#1589,#1055,.T.);
#1941=EDGE_CURVE('',#1591,#1591,#334,.T.);
#1942=EDGE_CURVE('',#1592,#1592,#335,.F.);
#1943=EDGE_CURVE('',#1592,#1591,#1056,.T.);
#1944=EDGE_CURVE('',#1593,#1593,#336,.F.);
#1945=EDGE_CURVE('',#1593,#1592,#1057,.T.);
#1946=EDGE_CURVE('',#1594,#1594,#337,.T.);
#1947=EDGE_CURVE('',#1594,#1593,#1058,.T.);
#1948=EDGE_CURVE('',#1595,#1596,#1059,.T.);
#1949=EDGE_CURVE('',#1596,#1597,#1060,.T.);
#1950=EDGE_CURVE('',#1597,#1598,#1061,.T.);
#1951=EDGE_CURVE('',#1595,#1598,#1062,.T.);
#1952=EDGE_CURVE('',#1596,#1599,#1063,.T.);
#1953=EDGE_CURVE('',#1599,#1600,#1064,.T.);
#1954=EDGE_CURVE('',#1600,#1597,#1065,.T.);
#1955=EDGE_CURVE('',#1599,#1601,#1066,.T.);
#1956=EDGE_CURVE('',#1601,#1602,#1067,.T.);
#1957=EDGE_CURVE('',#1602,#1600,#1068,.T.);
#1958=EDGE_CURVE('',#1601,#1603,#1069,.T.);
#1959=EDGE_CURVE('',#1603,#1604,#1070,.T.);
#1960=EDGE_CURVE('',#1604,#1602,#1071,.T.);
#1961=EDGE_CURVE('',#1603,#1605,#1072,.T.);
#1962=EDGE_CURVE('',#1605,#1606,#1073,.T.);
#1963=EDGE_CURVE('',#1606,#1604,#1074,.T.);
#1964=EDGE_CURVE('',#1605,#1595,#1075,.T.);
#1965=EDGE_CURVE('',#1598,#1606,#1076,.T.);
#1966=EDGE_CURVE('',#1607,#1607,#338,.T.);
#1967=EDGE_CURVE('',#1607,#1608,#1077,.T.);
#1968=EDGE_CURVE('',#1608,#1608,#339,.T.);
#1969=EDGE_CURVE('',#1609,#1609,#340,.T.);
#1970=EDGE_CURVE('',#1609,#1610,#1078,.T.);
#1971=EDGE_CURVE('',#1610,#1610,#341,.T.);
#1972=EDGE_CURVE('',#1611,#1611,#342,.T.);
#1973=EDGE_CURVE('',#1611,#1612,#1079,.T.);
#1974=EDGE_CURVE('',#1612,#1612,#343,.T.);
#1975=EDGE_CURVE('',#1613,#1613,#344,.T.);
#1976=EDGE_CURVE('',#1613,#1614,#1080,.T.);
#1977=EDGE_CURVE('',#1614,#1614,#345,.T.);
#1978=EDGE_CURVE('',#1615,#1616,#1081,.T.);
#1979=EDGE_CURVE('',#1616,#1617,#1082,.T.);
#1980=EDGE_CURVE('',#1618,#1617,#1083,.T.);
#1981=EDGE_CURVE('',#1615,#1618,#1084,.T.);
#1982=EDGE_CURVE('',#1619,#1615,#1085,.T.);
#1983=EDGE_CURVE('',#1620,#1618,#1086,.T.);
#1984=EDGE_CURVE('',#1619,#1620,#1087,.T.);
#1985=EDGE_CURVE('',#1621,#1619,#1088,.T.);
#1986=EDGE_CURVE('',#1622,#1620,#1089,.T.);
#1987=EDGE_CURVE('',#1621,#1622,#1090,.T.);
#1988=EDGE_CURVE('',#1616,#1621,#1091,.T.);
#1989=EDGE_CURVE('',#1617,#1622,#1092,.T.);
#1990=EDGE_CURVE('',#1623,#1623,#346,.T.);
#1991=EDGE_CURVE('',#1623,#1624,#1093,.T.);
#1992=EDGE_CURVE('',#1624,#1624,#347,.T.);
#1993=EDGE_CURVE('',#1625,#1625,#348,.T.);
#1994=EDGE_CURVE('',#1625,#1626,#1094,.T.);
#1995=EDGE_CURVE('',#1626,#1626,#349,.T.);
#1996=EDGE_CURVE('',#1627,#1628,#1095,.T.);
#1997=EDGE_CURVE('',#1629,#1627,#350,.T.);
#1998=EDGE_CURVE('',#1630,#1629,#1096,.T.);
#1999=EDGE_CURVE('',#1628,#1630,#351,.T.);
#2000=EDGE_CURVE('',#1627,#1631,#1097,.T.);
#2001=EDGE_CURVE('',#1632,#1631,#1098,.T.);
#2002=EDGE_CURVE('',#1629,#1632,#1099,.T.);
#2003=EDGE_CURVE('',#1628,#1633,#1100,.T.);
#2004=EDGE_CURVE('',#1631,#1633,#1101,.T.);
#2005=EDGE_CURVE('',#1634,#1632,#1102,.T.);
#2006=EDGE_CURVE('',#1630,#1634,#1103,.T.);
#2007=EDGE_CURVE('',#1633,#1634,#1104,.T.);
#2008=EDGE_CURVE('',#1635,#1635,#352,.T.);
#2009=EDGE_CURVE('',#1635,#1636,#1105,.T.);
#2010=EDGE_CURVE('',#1636,#1636,#353,.T.);
#2011=EDGE_CURVE('',#1637,#1638,#1106,.T.);
#2012=EDGE_CURVE('',#1638,#1639,#1107,.T.);
#2013=EDGE_CURVE('',#1639,#1640,#1108,.T.);
#2014=EDGE_CURVE('',#1637,#1640,#1109,.T.);
#2015=EDGE_CURVE('',#1638,#1641,#1110,.T.);
#2016=EDGE_CURVE('',#1641,#1642,#1111,.T.);
#2017=EDGE_CURVE('',#1642,#1639,#1112,.T.);
#2018=EDGE_CURVE('',#1641,#1643,#1113,.T.);
#2019=EDGE_CURVE('',#1643,#1644,#1114,.T.);
#2020=EDGE_CURVE('',#1644,#1642,#1115,.T.);
#2021=EDGE_CURVE('',#1643,#1645,#1116,.T.);
#2022=EDGE_CURVE('',#1645,#1646,#1117,.T.);
#2023=EDGE_CURVE('',#1646,#1644,#1118,.T.);
#2024=EDGE_CURVE('',#1645,#1647,#1119,.T.);
#2025=EDGE_CURVE('',#1647,#1648,#1120,.T.);
#2026=EDGE_CURVE('',#1648,#1646,#1121,.T.);
#2027=EDGE_CURVE('',#1647,#1637,#1122,.T.);
#2028=EDGE_CURVE('',#1640,#1648,#1123,.T.);
#2029=EDGE_CURVE('',#1649,#1649,#354,.T.);
#2030=EDGE_CURVE('',#1650,#1650,#355,.T.);
#2031=EDGE_CURVE('',#1651,#1651,#356,.T.);
#2032=EDGE_CURVE('',#1651,#1650,#1124,.T.);
#2033=EDGE_CURVE('',#1652,#1652,#357,.T.);
#2034=EDGE_CURVE('',#1652,#1651,#1125,.T.);
#2035=EDGE_CURVE('',#1653,#1653,#358,.T.);
#2036=EDGE_CURVE('',#1653,#1652,#1126,.T.);
#2037=EDGE_CURVE('',#1654,#1654,#359,.T.);
#2038=EDGE_CURVE('',#1655,#1655,#360,.F.);
#2039=EDGE_CURVE('',#1655,#1654,#1127,.T.);
#2040=EDGE_CURVE('',#1649,#1655,#1128,.T.);
#2041=EDGE_CURVE('',#1656,#1656,#361,.F.);
#2042=EDGE_CURVE('',#1656,#1657,#1129,.T.);
#2043=EDGE_CURVE('',#1657,#1657,#362,.F.);
#2044=EDGE_CURVE('',#1658,#1658,#363,.T.);
#2045=EDGE_CURVE('',#1658,#1659,#1130,.T.);
#2046=EDGE_CURVE('',#1659,#1659,#364,.T.);
#2047=EDGE_CURVE('',#1660,#1660,#365,.T.);
#2048=EDGE_CURVE('',#1660,#1661,#1131,.T.);
#2049=EDGE_CURVE('',#1661,#1661,#366,.T.);
#2050=EDGE_CURVE('',#1662,#1663,#115,.T.);
#2051=EDGE_CURVE('',#1664,#1662,#116,.T.);
#2052=EDGE_CURVE('',#1664,#1665,#1132,.T.);
#2053=EDGE_CURVE('',#1665,#1665,#367,.T.);
#2054=EDGE_CURVE('',#1666,#1664,#117,.T.);
#2055=EDGE_CURVE('',#1667,#1666,#118,.T.);
#2056=EDGE_CURVE('',#1668,#1667,#119,.T.);
#2057=EDGE_CURVE('',#1663,#1668,#120,.T.);
#2058=EDGE_CURVE('',#1669,#1669,#368,.T.);
#2059=EDGE_CURVE('',#1669,#1670,#1133,.T.);
#2060=EDGE_CURVE('',#1671,#1670,#121,.T.);
#2061=EDGE_CURVE('',#1672,#1671,#122,.T.);
#2062=EDGE_CURVE('',#1673,#1672,#123,.T.);
#2063=EDGE_CURVE('',#1674,#1673,#124,.T.);
#2064=EDGE_CURVE('',#1675,#1674,#125,.T.);
#2065=EDGE_CURVE('',#1670,#1675,#126,.T.);
#2066=EDGE_CURVE('',#1666,#1675,#1134,.T.);
#2067=EDGE_CURVE('',#1667,#1674,#1135,.T.);
#2068=EDGE_CURVE('',#1664,#1670,#1136,.T.);
#2069=EDGE_CURVE('',#1662,#1671,#1137,.T.);
#2070=EDGE_CURVE('',#1676,#1676,#369,.F.);
#2071=EDGE_CURVE('',#1676,#1677,#1138,.T.);
#2072=EDGE_CURVE('',#1677,#1677,#370,.F.);
#2073=EDGE_CURVE('',#1663,#1672,#1139,.T.);
#2074=EDGE_CURVE('',#1668,#1673,#1140,.T.);
#2075=EDGE_CURVE('',#1678,#1679,#1141,.T.);
#2076=EDGE_CURVE('',#1680,#1678,#371,.T.);
#2077=EDGE_CURVE('',#1681,#1680,#1142,.T.);
#2078=EDGE_CURVE('',#1679,#1681,#372,.T.);
#2079=EDGE_CURVE('',#1682,#1683,#1143,.T.);
#2080=EDGE_CURVE('',#1684,#1682,#373,.T.);
#2081=EDGE_CURVE('',#1685,#1684,#1144,.T.);
#2082=EDGE_CURVE('',#1683,#1685,#374,.T.);
#2083=EDGE_CURVE('',#1686,#1687,#1145,.T.);
#2084=EDGE_CURVE('',#1688,#1686,#375,.T.);
#2085=EDGE_CURVE('',#1689,#1688,#1146,.T.);
#2086=EDGE_CURVE('',#1687,#1689,#376,.T.);
#2087=EDGE_CURVE('',#1690,#1691,#1147,.T.);
#2088=EDGE_CURVE('',#1692,#1690,#377,.T.);
#2089=EDGE_CURVE('',#1693,#1692,#1148,.T.);
#2090=EDGE_CURVE('',#1691,#1693,#378,.T.);
#2091=EDGE_CURVE('',#1694,#1695,#1149,.T.);
#2092=EDGE_CURVE('',#1696,#1694,#379,.T.);
#2093=EDGE_CURVE('',#1697,#1696,#1150,.T.);
#2094=EDGE_CURVE('',#1695,#1697,#380,.T.);
#2095=EDGE_CURVE('',#1698,#1699,#1151,.T.);
#2096=EDGE_CURVE('',#1700,#1698,#381,.T.);
#2097=EDGE_CURVE('',#1701,#1700,#1152,.T.);
#2098=EDGE_CURVE('',#1699,#1701,#382,.T.);
#2099=EDGE_CURVE('',#1678,#1700,#383,.T.);
#2100=EDGE_CURVE('',#1698,#1683,#384,.T.);
#2101=EDGE_CURVE('',#1685,#1688,#385,.T.);
#2102=EDGE_CURVE('',#1686,#1692,#386,.T.);
#2103=EDGE_CURVE('',#1690,#1696,#387,.T.);
#2104=EDGE_CURVE('',#1694,#1680,#388,.T.);
#2105=EDGE_CURVE('',#1702,#1702,#389,.T.);
#2106=EDGE_CURVE('',#1691,#1697,#390,.T.);
#2107=EDGE_CURVE('',#1687,#1693,#391,.T.);
#2108=EDGE_CURVE('',#1699,#1682,#392,.T.);
#2109=EDGE_CURVE('',#1684,#1689,#393,.T.);
#2110=EDGE_CURVE('',#1679,#1701,#394,.T.);
#2111=EDGE_CURVE('',#1695,#1681,#395,.T.);
#2112=EDGE_CURVE('',#1703,#1704,#1153,.T.);
#2113=EDGE_CURVE('',#1703,#1705,#1154,.T.);
#2114=EDGE_CURVE('',#1705,#1706,#1155,.T.);
#2115=EDGE_CURVE('',#1704,#1706,#1156,.T.);
#2116=EDGE_CURVE('',#1704,#1707,#1157,.T.);
#2117=EDGE_CURVE('',#1706,#1708,#1158,.T.);
#2118=EDGE_CURVE('',#1707,#1708,#1159,.T.);
#2119=EDGE_CURVE('',#1707,#1709,#1160,.T.);
#2120=EDGE_CURVE('',#1708,#1710,#1161,.T.);
#2121=EDGE_CURVE('',#1709,#1710,#1162,.T.);
#2122=EDGE_CURVE('',#1709,#1711,#1163,.T.);
#2123=EDGE_CURVE('',#1710,#1712,#1164,.T.);
#2124=EDGE_CURVE('',#1711,#1712,#1165,.T.);
#2125=EDGE_CURVE('',#1713,#1703,#1166,.T.);
#2126=EDGE_CURVE('',#1713,#1714,#1167,.T.);
#2127=EDGE_CURVE('',#1714,#1705,#1168,.T.);
#2128=EDGE_CURVE('',#1711,#1713,#1169,.T.);
#2129=EDGE_CURVE('',#1712,#1714,#1170,.T.);
#2130=EDGE_CURVE('',#1715,#1715,#396,.T.);
#2131=EDGE_CURVE('',#1702,#1715,#1171,.T.);
#2132=ORIENTED_EDGE('',*,*,#1716,.F.);
#2133=ORIENTED_EDGE('',*,*,#1717,.F.);
#2134=ORIENTED_EDGE('',*,*,#1718,.F.);
#2135=ORIENTED_EDGE('',*,*,#1719,.T.);
#2136=ORIENTED_EDGE('',*,*,#1720,.F.);
#2137=ORIENTED_EDGE('',*,*,#1719,.F.);
#2138=ORIENTED_EDGE('',*,*,#1721,.F.);
#2139=ORIENTED_EDGE('',*,*,#1722,.T.);
#2140=ORIENTED_EDGE('',*,*,#1723,.F.);
#2141=ORIENTED_EDGE('',*,*,#1722,.F.);
#2142=ORIENTED_EDGE('',*,*,#1724,.F.);
#2143=ORIENTED_EDGE('',*,*,#1725,.T.);
#2144=ORIENTED_EDGE('',*,*,#1726,.F.);
#2145=ORIENTED_EDGE('',*,*,#1725,.F.);
#2146=ORIENTED_EDGE('',*,*,#1727,.F.);
#2147=ORIENTED_EDGE('',*,*,#1717,.T.);
#2148=ORIENTED_EDGE('',*,*,#1721,.T.);
#2149=ORIENTED_EDGE('',*,*,#1718,.T.);
#2150=ORIENTED_EDGE('',*,*,#1727,.T.);
#2151=ORIENTED_EDGE('',*,*,#1724,.T.);
#2152=ORIENTED_EDGE('',*,*,#1728,.F.);
#2153=ORIENTED_EDGE('',*,*,#1729,.F.);
#2154=ORIENTED_EDGE('',*,*,#1730,.F.);
#2155=ORIENTED_EDGE('',*,*,#1731,.T.);
#2156=ORIENTED_EDGE('',*,*,#1732,.F.);
#2157=ORIENTED_EDGE('',*,*,#1731,.F.);
#2158=ORIENTED_EDGE('',*,*,#1733,.F.);
#2159=ORIENTED_EDGE('',*,*,#1734,.T.);
#2160=ORIENTED_EDGE('',*,*,#1735,.F.);
#2161=ORIENTED_EDGE('',*,*,#1734,.F.);
#2162=ORIENTED_EDGE('',*,*,#1736,.F.);
#2163=ORIENTED_EDGE('',*,*,#1737,.T.);
#2164=ORIENTED_EDGE('',*,*,#1738,.F.);
#2165=ORIENTED_EDGE('',*,*,#1737,.F.);
#2166=ORIENTED_EDGE('',*,*,#1739,.F.);
#2167=ORIENTED_EDGE('',*,*,#1729,.T.);
#2168=ORIENTED_EDGE('',*,*,#1733,.T.);
#2169=ORIENTED_EDGE('',*,*,#1730,.T.);
#2170=ORIENTED_EDGE('',*,*,#1739,.T.);
#2171=ORIENTED_EDGE('',*,*,#1736,.T.);
#2172=ORIENTED_EDGE('',*,*,#1740,.F.);
#2173=ORIENTED_EDGE('',*,*,#1741,.T.);
#2174=ORIENTED_EDGE('',*,*,#1742,.F.);
#2175=ORIENTED_EDGE('',*,*,#1741,.F.);
#2176=ORIENTED_EDGE('',*,*,#1743,.F.);
#2177=ORIENTED_EDGE('',*,*,#1744,.T.);
#2178=ORIENTED_EDGE('',*,*,#1745,.F.);
#2179=ORIENTED_EDGE('',*,*,#1744,.F.);
#2180=ORIENTED_EDGE('',*,*,#1746,.F.);
#2181=ORIENTED_EDGE('',*,*,#1747,.T.);
#2182=ORIENTED_EDGE('',*,*,#1748,.F.);
#2183=ORIENTED_EDGE('',*,*,#1747,.F.);
#2184=ORIENTED_EDGE('',*,*,#1749,.F.);
#2185=ORIENTED_EDGE('',*,*,#1750,.T.);
#2186=ORIENTED_EDGE('',*,*,#1751,.F.);
#2187=ORIENTED_EDGE('',*,*,#1750,.F.);
#2188=ORIENTED_EDGE('',*,*,#1752,.F.);
#2189=ORIENTED_EDGE('',*,*,#1753,.T.);
#2190=ORIENTED_EDGE('',*,*,#1754,.F.);
#2191=ORIENTED_EDGE('',*,*,#1753,.F.);
#2192=ORIENTED_EDGE('',*,*,#1755,.F.);
#2193=ORIENTED_EDGE('',*,*,#1756,.T.);
#2194=ORIENTED_EDGE('',*,*,#1757,.F.);
#2195=ORIENTED_EDGE('',*,*,#1756,.F.);
#2196=ORIENTED_EDGE('',*,*,#1758,.F.);
#2197=ORIENTED_EDGE('',*,*,#1759,.T.);
#2198=ORIENTED_EDGE('',*,*,#1760,.F.);
#2199=ORIENTED_EDGE('',*,*,#1759,.F.);
#2200=ORIENTED_EDGE('',*,*,#1761,.F.);
#2201=ORIENTED_EDGE('',*,*,#1762,.T.);
#2202=ORIENTED_EDGE('',*,*,#1763,.F.);
#2203=ORIENTED_EDGE('',*,*,#1762,.F.);
#2204=ORIENTED_EDGE('',*,*,#1764,.F.);
#2205=ORIENTED_EDGE('',*,*,#1765,.T.);
#2206=ORIENTED_EDGE('',*,*,#1766,.F.);
#2207=ORIENTED_EDGE('',*,*,#1765,.F.);
#2208=ORIENTED_EDGE('',*,*,#1767,.F.);
#2209=ORIENTED_EDGE('',*,*,#1768,.T.);
#2210=ORIENTED_EDGE('',*,*,#1769,.F.);
#2211=ORIENTED_EDGE('',*,*,#1768,.F.);
#2212=ORIENTED_EDGE('',*,*,#1770,.F.);
#2213=ORIENTED_EDGE('',*,*,#1771,.T.);
#2214=ORIENTED_EDGE('',*,*,#1772,.F.);
#2215=ORIENTED_EDGE('',*,*,#1771,.F.);
#2216=ORIENTED_EDGE('',*,*,#1773,.F.);
#2217=ORIENTED_EDGE('',*,*,#1774,.T.);
#2218=ORIENTED_EDGE('',*,*,#1775,.F.);
#2219=ORIENTED_EDGE('',*,*,#1774,.F.);
#2220=ORIENTED_EDGE('',*,*,#1776,.F.);
#2221=ORIENTED_EDGE('',*,*,#1777,.T.);
#2222=ORIENTED_EDGE('',*,*,#1778,.F.);
#2223=ORIENTED_EDGE('',*,*,#1777,.F.);
#2224=ORIENTED_EDGE('',*,*,#1779,.F.);
#2225=ORIENTED_EDGE('',*,*,#1780,.T.);
#2226=ORIENTED_EDGE('',*,*,#1781,.F.);
#2227=ORIENTED_EDGE('',*,*,#1780,.F.);
#2228=ORIENTED_EDGE('',*,*,#1782,.F.);
#2229=ORIENTED_EDGE('',*,*,#1783,.T.);
#2230=ORIENTED_EDGE('',*,*,#1784,.F.);
#2231=ORIENTED_EDGE('',*,*,#1783,.F.);
#2232=ORIENTED_EDGE('',*,*,#1785,.F.);
#2233=ORIENTED_EDGE('',*,*,#1786,.T.);
#2234=ORIENTED_EDGE('',*,*,#1787,.F.);
#2235=ORIENTED_EDGE('',*,*,#1786,.F.);
#2236=ORIENTED_EDGE('',*,*,#1788,.F.);
#2237=ORIENTED_EDGE('',*,*,#1789,.T.);
#2238=ORIENTED_EDGE('',*,*,#1790,.F.);
#2239=ORIENTED_EDGE('',*,*,#1789,.F.);
#2240=ORIENTED_EDGE('',*,*,#1791,.F.);
#2241=ORIENTED_EDGE('',*,*,#1792,.T.);
#2242=ORIENTED_EDGE('',*,*,#1793,.F.);
#2243=ORIENTED_EDGE('',*,*,#1792,.F.);
#2244=ORIENTED_EDGE('',*,*,#1794,.F.);
#2245=ORIENTED_EDGE('',*,*,#1795,.T.);
#2246=ORIENTED_EDGE('',*,*,#1796,.F.);
#2247=ORIENTED_EDGE('',*,*,#1795,.F.);
#2248=ORIENTED_EDGE('',*,*,#1797,.F.);
#2249=ORIENTED_EDGE('',*,*,#1798,.T.);
#2250=ORIENTED_EDGE('',*,*,#1799,.F.);
#2251=ORIENTED_EDGE('',*,*,#1798,.F.);
#2252=ORIENTED_EDGE('',*,*,#1800,.F.);
#2253=ORIENTED_EDGE('',*,*,#1801,.T.);
#2254=ORIENTED_EDGE('',*,*,#1802,.F.);
#2255=ORIENTED_EDGE('',*,*,#1801,.F.);
#2256=ORIENTED_EDGE('',*,*,#1803,.F.);
#2257=ORIENTED_EDGE('',*,*,#1804,.T.);
#2258=ORIENTED_EDGE('',*,*,#1805,.F.);
#2259=ORIENTED_EDGE('',*,*,#1804,.F.);
#2260=ORIENTED_EDGE('',*,*,#1806,.F.);
#2261=ORIENTED_EDGE('',*,*,#1807,.T.);
#2262=ORIENTED_EDGE('',*,*,#1808,.F.);
#2263=ORIENTED_EDGE('',*,*,#1807,.F.);
#2264=ORIENTED_EDGE('',*,*,#1809,.F.);
#2265=ORIENTED_EDGE('',*,*,#1810,.T.);
#2266=ORIENTED_EDGE('',*,*,#1811,.F.);
#2267=ORIENTED_EDGE('',*,*,#1810,.F.);
#2268=ORIENTED_EDGE('',*,*,#1812,.F.);
#2269=ORIENTED_EDGE('',*,*,#1813,.T.);
#2270=ORIENTED_EDGE('',*,*,#1814,.F.);
#2271=ORIENTED_EDGE('',*,*,#1813,.F.);
#2272=ORIENTED_EDGE('',*,*,#1815,.T.);
#2273=ORIENTED_EDGE('',*,*,#1816,.T.);
#2274=ORIENTED_EDGE('',*,*,#1817,.F.);
#2275=ORIENTED_EDGE('',*,*,#1818,.F.);
#2276=ORIENTED_EDGE('',*,*,#1819,.T.);
#2277=ORIENTED_EDGE('',*,*,#1818,.T.);
#2278=ORIENTED_EDGE('',*,*,#1820,.F.);
#2279=ORIENTED_EDGE('',*,*,#1821,.F.);
#2280=ORIENTED_EDGE('',*,*,#1822,.T.);
#2281=ORIENTED_EDGE('',*,*,#1821,.T.);
#2282=ORIENTED_EDGE('',*,*,#1823,.F.);
#2283=ORIENTED_EDGE('',*,*,#1824,.F.);
#2284=ORIENTED_EDGE('',*,*,#1825,.T.);
#2285=ORIENTED_EDGE('',*,*,#1824,.T.);
#2286=ORIENTED_EDGE('',*,*,#1826,.F.);
#2287=ORIENTED_EDGE('',*,*,#1816,.F.);
#2288=ORIENTED_EDGE('',*,*,#1826,.T.);
#2289=ORIENTED_EDGE('',*,*,#1823,.T.);
#2290=ORIENTED_EDGE('',*,*,#1820,.T.);
#2291=ORIENTED_EDGE('',*,*,#1817,.T.);
#2292=ORIENTED_EDGE('',*,*,#1735,.T.);
#2293=ORIENTED_EDGE('',*,*,#1738,.T.);
#2294=ORIENTED_EDGE('',*,*,#1728,.T.);
#2295=ORIENTED_EDGE('',*,*,#1732,.T.);
#2296=ORIENTED_EDGE('',*,*,#1754,.T.);
#2297=ORIENTED_EDGE('',*,*,#1757,.T.);
#2298=ORIENTED_EDGE('',*,*,#1814,.T.);
#2299=ORIENTED_EDGE('',*,*,#1811,.T.);
#2300=ORIENTED_EDGE('',*,*,#1808,.T.);
#2301=ORIENTED_EDGE('',*,*,#1805,.T.);
#2302=ORIENTED_EDGE('',*,*,#1802,.T.);
#2303=ORIENTED_EDGE('',*,*,#1799,.T.);
#2304=ORIENTED_EDGE('',*,*,#1796,.T.);
#2305=ORIENTED_EDGE('',*,*,#1793,.T.);
#2306=ORIENTED_EDGE('',*,*,#1790,.T.);
#2307=ORIENTED_EDGE('',*,*,#1787,.T.);
#2308=ORIENTED_EDGE('',*,*,#1784,.T.);
#2309=ORIENTED_EDGE('',*,*,#1781,.T.);
#2310=ORIENTED_EDGE('',*,*,#1778,.T.);
#2311=ORIENTED_EDGE('',*,*,#1775,.T.);
#2312=ORIENTED_EDGE('',*,*,#1772,.T.);
#2313=ORIENTED_EDGE('',*,*,#1769,.T.);
#2314=ORIENTED_EDGE('',*,*,#1766,.T.);
#2315=ORIENTED_EDGE('',*,*,#1763,.T.);
#2316=ORIENTED_EDGE('',*,*,#1760,.T.);
#2317=ORIENTED_EDGE('',*,*,#1751,.T.);
#2318=ORIENTED_EDGE('',*,*,#1748,.T.);
#2319=ORIENTED_EDGE('',*,*,#1745,.T.);
#2320=ORIENTED_EDGE('',*,*,#1742,.T.);
#2321=ORIENTED_EDGE('',*,*,#1723,.T.);
#2322=ORIENTED_EDGE('',*,*,#1726,.T.);
#2323=ORIENTED_EDGE('',*,*,#1716,.T.);
#2324=ORIENTED_EDGE('',*,*,#1720,.T.);
#2325=ORIENTED_EDGE('',*,*,#1825,.F.);
#2326=ORIENTED_EDGE('',*,*,#1815,.F.);
#2327=ORIENTED_EDGE('',*,*,#1819,.F.);
#2328=ORIENTED_EDGE('',*,*,#1822,.F.);
#2329=ORIENTED_EDGE('',*,*,#1752,.T.);
#2330=ORIENTED_EDGE('',*,*,#1755,.T.);
#2331=ORIENTED_EDGE('',*,*,#1812,.T.);
#2332=ORIENTED_EDGE('',*,*,#1809,.T.);
#2333=ORIENTED_EDGE('',*,*,#1806,.T.);
#2334=ORIENTED_EDGE('',*,*,#1803,.T.);
#2335=ORIENTED_EDGE('',*,*,#1800,.T.);
#2336=ORIENTED_EDGE('',*,*,#1797,.T.);
#2337=ORIENTED_EDGE('',*,*,#1794,.T.);
#2338=ORIENTED_EDGE('',*,*,#1791,.T.);
#2339=ORIENTED_EDGE('',*,*,#1788,.T.);
#2340=ORIENTED_EDGE('',*,*,#1785,.T.);
#2341=ORIENTED_EDGE('',*,*,#1782,.T.);
#2342=ORIENTED_EDGE('',*,*,#1779,.T.);
#2343=ORIENTED_EDGE('',*,*,#1776,.T.);
#2344=ORIENTED_EDGE('',*,*,#1773,.T.);
#2345=ORIENTED_EDGE('',*,*,#1770,.T.);
#2346=ORIENTED_EDGE('',*,*,#1767,.T.);
#2347=ORIENTED_EDGE('',*,*,#1764,.T.);
#2348=ORIENTED_EDGE('',*,*,#1761,.T.);
#2349=ORIENTED_EDGE('',*,*,#1758,.T.);
#2350=ORIENTED_EDGE('',*,*,#1749,.T.);
#2351=ORIENTED_EDGE('',*,*,#1746,.T.);
#2352=ORIENTED_EDGE('',*,*,#1743,.T.);
#2353=ORIENTED_EDGE('',*,*,#1740,.T.);
#2354=ORIENTED_EDGE('',*,*,#1827,.F.);
#2355=ORIENTED_EDGE('',*,*,#1828,.F.);
#2356=ORIENTED_EDGE('',*,*,#1829,.F.);
#2357=ORIENTED_EDGE('',*,*,#1830,.F.);
#2358=ORIENTED_EDGE('',*,*,#1831,.F.);
#2359=ORIENTED_EDGE('',*,*,#1832,.F.);
#2360=ORIENTED_EDGE('',*,*,#1833,.F.);
#2361=ORIENTED_EDGE('',*,*,#1834,.F.);
#2362=ORIENTED_EDGE('',*,*,#1831,.T.);
#2363=ORIENTED_EDGE('',*,*,#1835,.T.);
#2364=ORIENTED_EDGE('',*,*,#1836,.T.);
#2365=ORIENTED_EDGE('',*,*,#1837,.T.);
#2366=ORIENTED_EDGE('',*,*,#1830,.T.);
#2367=ORIENTED_EDGE('',*,*,#1838,.F.);
#2368=ORIENTED_EDGE('',*,*,#1839,.T.);
#2369=ORIENTED_EDGE('',*,*,#1835,.F.);
#2370=ORIENTED_EDGE('',*,*,#1829,.T.);
#2371=ORIENTED_EDGE('',*,*,#1840,.T.);
#2372=ORIENTED_EDGE('',*,*,#1841,.T.);
#2373=ORIENTED_EDGE('',*,*,#1838,.T.);
#2374=ORIENTED_EDGE('',*,*,#1828,.T.);
#2375=ORIENTED_EDGE('',*,*,#1842,.F.);
#2376=ORIENTED_EDGE('',*,*,#1843,.T.);
#2377=ORIENTED_EDGE('',*,*,#1840,.F.);
#2378=ORIENTED_EDGE('',*,*,#1844,.F.);
#2379=ORIENTED_EDGE('',*,*,#1845,.F.);
#2380=ORIENTED_EDGE('',*,*,#1836,.F.);
#2381=ORIENTED_EDGE('',*,*,#1839,.F.);
#2382=ORIENTED_EDGE('',*,*,#1841,.F.);
#2383=ORIENTED_EDGE('',*,*,#1843,.F.);
#2384=ORIENTED_EDGE('',*,*,#1846,.F.);
#2385=ORIENTED_EDGE('',*,*,#1847,.F.);
#2386=ORIENTED_EDGE('',*,*,#1832,.T.);
#2387=ORIENTED_EDGE('',*,*,#1837,.F.);
#2388=ORIENTED_EDGE('',*,*,#1845,.T.);
#2389=ORIENTED_EDGE('',*,*,#1848,.F.);
#2390=ORIENTED_EDGE('',*,*,#1827,.T.);
#2391=ORIENTED_EDGE('',*,*,#1849,.T.);
#2392=ORIENTED_EDGE('',*,*,#1846,.T.);
#2393=ORIENTED_EDGE('',*,*,#1842,.T.);
#2394=ORIENTED_EDGE('',*,*,#1833,.T.);
#2395=ORIENTED_EDGE('',*,*,#1848,.T.);
#2396=ORIENTED_EDGE('',*,*,#1844,.T.);
#2397=ORIENTED_EDGE('',*,*,#1850,.T.);
#2398=ORIENTED_EDGE('',*,*,#1834,.T.);
#2399=ORIENTED_EDGE('',*,*,#1850,.F.);
#2400=ORIENTED_EDGE('',*,*,#1847,.T.);
#2401=ORIENTED_EDGE('',*,*,#1849,.F.);
#2402=ORIENTED_EDGE('',*,*,#1851,.F.);
#2403=ORIENTED_EDGE('',*,*,#1852,.F.);
#2404=ORIENTED_EDGE('',*,*,#1853,.T.);
#2405=ORIENTED_EDGE('',*,*,#1854,.F.);
#2406=ORIENTED_EDGE('',*,*,#1855,.F.);
#2407=ORIENTED_EDGE('',*,*,#1856,.F.);
#2408=ORIENTED_EDGE('',*,*,#1857,.T.);
#2409=ORIENTED_EDGE('',*,*,#1858,.F.);
#2410=ORIENTED_EDGE('',*,*,#1859,.F.);
#2411=ORIENTED_EDGE('',*,*,#1860,.F.);
#2412=ORIENTED_EDGE('',*,*,#1861,.T.);
#2413=ORIENTED_EDGE('',*,*,#1862,.T.);
#2414=ORIENTED_EDGE('',*,*,#1863,.F.);
#2415=ORIENTED_EDGE('',*,*,#1864,.F.);
#2416=ORIENTED_EDGE('',*,*,#1863,.T.);
#2417=ORIENTED_EDGE('',*,*,#1865,.T.);
#2418=ORIENTED_EDGE('',*,*,#1866,.F.);
#2419=ORIENTED_EDGE('',*,*,#1867,.F.);
#2420=ORIENTED_EDGE('',*,*,#1866,.T.);
#2421=ORIENTED_EDGE('',*,*,#1868,.T.);
#2422=ORIENTED_EDGE('',*,*,#1869,.F.);
#2423=ORIENTED_EDGE('',*,*,#1870,.F.);
#2424=ORIENTED_EDGE('',*,*,#1869,.T.);
#2425=ORIENTED_EDGE('',*,*,#1871,.T.);
#2426=ORIENTED_EDGE('',*,*,#1861,.F.);
#2427=ORIENTED_EDGE('',*,*,#1871,.F.);
#2428=ORIENTED_EDGE('',*,*,#1868,.F.);
#2429=ORIENTED_EDGE('',*,*,#1865,.F.);
#2430=ORIENTED_EDGE('',*,*,#1862,.F.);
#2431=ORIENTED_EDGE('',*,*,#1855,.T.);
#2432=ORIENTED_EDGE('',*,*,#1872,.F.);
#2433=ORIENTED_EDGE('',*,*,#1873,.F.);
#2434=ORIENTED_EDGE('',*,*,#1874,.F.);
#2435=ORIENTED_EDGE('',*,*,#1856,.T.);
#2436=ORIENTED_EDGE('',*,*,#1874,.T.);
#2437=ORIENTED_EDGE('',*,*,#1875,.F.);
#2438=ORIENTED_EDGE('',*,*,#1851,.T.);
#2439=ORIENTED_EDGE('',*,*,#1876,.F.);
#2440=ORIENTED_EDGE('',*,*,#1877,.F.);
#2441=ORIENTED_EDGE('',*,*,#1878,.F.);
#2442=ORIENTED_EDGE('',*,*,#1879,.F.);
#2443=ORIENTED_EDGE('',*,*,#1852,.T.);
#2444=ORIENTED_EDGE('',*,*,#1879,.T.);
#2445=ORIENTED_EDGE('',*,*,#1880,.F.);
#2446=ORIENTED_EDGE('',*,*,#1859,.T.);
#2447=ORIENTED_EDGE('',*,*,#1881,.F.);
#2448=ORIENTED_EDGE('',*,*,#1882,.F.);
#2449=ORIENTED_EDGE('',*,*,#1883,.F.);
#2450=ORIENTED_EDGE('',*,*,#1884,.F.);
#2451=ORIENTED_EDGE('',*,*,#1885,.F.);
#2452=ORIENTED_EDGE('',*,*,#1858,.T.);
#2453=ORIENTED_EDGE('',*,*,#1886,.T.);
#2454=ORIENTED_EDGE('',*,*,#1887,.T.);
#2455=ORIENTED_EDGE('',*,*,#1881,.T.);
#2456=ORIENTED_EDGE('',*,*,#1876,.T.);
#2457=ORIENTED_EDGE('',*,*,#1888,.F.);
#2458=ORIENTED_EDGE('',*,*,#1889,.F.);
#2459=ORIENTED_EDGE('',*,*,#1883,.T.);
#2460=ORIENTED_EDGE('',*,*,#1890,.F.);
#2461=ORIENTED_EDGE('',*,*,#1891,.F.);
#2462=ORIENTED_EDGE('',*,*,#1854,.T.);
#2463=ORIENTED_EDGE('',*,*,#1892,.T.);
#2464=ORIENTED_EDGE('',*,*,#1893,.T.);
#2465=ORIENTED_EDGE('',*,*,#1888,.T.);
#2466=ORIENTED_EDGE('',*,*,#1894,.F.);
#2467=ORIENTED_EDGE('',*,*,#1895,.T.);
#2468=ORIENTED_EDGE('',*,*,#1875,.T.);
#2469=ORIENTED_EDGE('',*,*,#1895,.F.);
#2470=ORIENTED_EDGE('',*,*,#1896,.F.);
#2471=ORIENTED_EDGE('',*,*,#1897,.T.);
#2472=ORIENTED_EDGE('',*,*,#1880,.T.);
#2473=ORIENTED_EDGE('',*,*,#1897,.F.);
#2474=ORIENTED_EDGE('',*,*,#1872,.T.);
#2475=ORIENTED_EDGE('',*,*,#1885,.T.);
#2476=ORIENTED_EDGE('',*,*,#1898,.T.);
#2477=ORIENTED_EDGE('',*,*,#1899,.T.);
#2478=ORIENTED_EDGE('',*,*,#1877,.T.);
#2479=ORIENTED_EDGE('',*,*,#1891,.T.);
#2480=ORIENTED_EDGE('',*,*,#1900,.T.);
#2481=ORIENTED_EDGE('',*,*,#1901,.T.);
#2482=ORIENTED_EDGE('',*,*,#1884,.T.);
#2483=ORIENTED_EDGE('',*,*,#1889,.T.);
#2484=ORIENTED_EDGE('',*,*,#1893,.F.);
#2485=ORIENTED_EDGE('',*,*,#1902,.F.);
#2486=ORIENTED_EDGE('',*,*,#1903,.T.);
#2487=ORIENTED_EDGE('',*,*,#1904,.T.);
#2488=ORIENTED_EDGE('',*,*,#1898,.F.);
#2489=ORIENTED_EDGE('',*,*,#1905,.T.);
#2490=ORIENTED_EDGE('',*,*,#1902,.T.);
#2491=ORIENTED_EDGE('',*,*,#1892,.F.);
#2492=ORIENTED_EDGE('',*,*,#1853,.F.);
#2493=ORIENTED_EDGE('',*,*,#1878,.T.);
#2494=ORIENTED_EDGE('',*,*,#1901,.F.);
#2495=ORIENTED_EDGE('',*,*,#1906,.F.);
#2496=ORIENTED_EDGE('',*,*,#1882,.T.);
#2497=ORIENTED_EDGE('',*,*,#1887,.F.);
#2498=ORIENTED_EDGE('',*,*,#1907,.F.);
#2499=ORIENTED_EDGE('',*,*,#1908,.T.);
#2500=ORIENTED_EDGE('',*,*,#1906,.T.);
#2501=ORIENTED_EDGE('',*,*,#1900,.F.);
#2502=ORIENTED_EDGE('',*,*,#1890,.T.);
#2503=ORIENTED_EDGE('',*,*,#1909,.T.);
#2504=ORIENTED_EDGE('',*,*,#1907,.T.);
#2505=ORIENTED_EDGE('',*,*,#1886,.F.);
#2506=ORIENTED_EDGE('',*,*,#1857,.F.);
#2507=ORIENTED_EDGE('',*,*,#1873,.T.);
#2508=ORIENTED_EDGE('',*,*,#1899,.F.);
#2509=ORIENTED_EDGE('',*,*,#1904,.F.);
#2510=ORIENTED_EDGE('',*,*,#1903,.F.);
#2511=ORIENTED_EDGE('',*,*,#1905,.F.);
#2512=ORIENTED_EDGE('',*,*,#1908,.F.);
#2513=ORIENTED_EDGE('',*,*,#1909,.F.);
#2514=ORIENTED_EDGE('',*,*,#1867,.T.);
#2515=ORIENTED_EDGE('',*,*,#1870,.T.);
#2516=ORIENTED_EDGE('',*,*,#1860,.T.);
#2517=ORIENTED_EDGE('',*,*,#1864,.T.);
#2518=ORIENTED_EDGE('',*,*,#1894,.T.);
#2519=ORIENTED_EDGE('',*,*,#1896,.T.);
#2520=ORIENTED_EDGE('',*,*,#1910,.T.);
#2521=ORIENTED_EDGE('',*,*,#1911,.T.);
#2522=ORIENTED_EDGE('',*,*,#1912,.F.);
#2523=ORIENTED_EDGE('',*,*,#1913,.F.);
#2524=ORIENTED_EDGE('',*,*,#1914,.T.);
#2525=ORIENTED_EDGE('',*,*,#1913,.T.);
#2526=ORIENTED_EDGE('',*,*,#1915,.F.);
#2527=ORIENTED_EDGE('',*,*,#1916,.F.);
#2528=ORIENTED_EDGE('',*,*,#1917,.T.);
#2529=ORIENTED_EDGE('',*,*,#1916,.T.);
#2530=ORIENTED_EDGE('',*,*,#1918,.F.);
#2531=ORIENTED_EDGE('',*,*,#1919,.F.);
#2532=ORIENTED_EDGE('',*,*,#1920,.T.);
#2533=ORIENTED_EDGE('',*,*,#1919,.T.);
#2534=ORIENTED_EDGE('',*,*,#1921,.F.);
#2535=ORIENTED_EDGE('',*,*,#1911,.F.);
#2536=ORIENTED_EDGE('',*,*,#1921,.T.);
#2537=ORIENTED_EDGE('',*,*,#1918,.T.);
#2538=ORIENTED_EDGE('',*,*,#1915,.T.);
#2539=ORIENTED_EDGE('',*,*,#1912,.T.);
#2540=ORIENTED_EDGE('',*,*,#1920,.F.);
#2541=ORIENTED_EDGE('',*,*,#1910,.F.);
#2542=ORIENTED_EDGE('',*,*,#1914,.F.);
#2543=ORIENTED_EDGE('',*,*,#1917,.F.);
#2544=ORIENTED_EDGE('',*,*,#1922,.T.);
#2545=ORIENTED_EDGE('',*,*,#1923,.T.);
#2546=ORIENTED_EDGE('',*,*,#1924,.F.);
#2547=ORIENTED_EDGE('',*,*,#1925,.F.);
#2548=ORIENTED_EDGE('',*,*,#1926,.T.);
#2549=ORIENTED_EDGE('',*,*,#1925,.T.);
#2550=ORIENTED_EDGE('',*,*,#1927,.F.);
#2551=ORIENTED_EDGE('',*,*,#1928,.F.);
#2552=ORIENTED_EDGE('',*,*,#1929,.T.);
#2553=ORIENTED_EDGE('',*,*,#1928,.T.);
#2554=ORIENTED_EDGE('',*,*,#1930,.F.);
#2555=ORIENTED_EDGE('',*,*,#1931,.F.);
#2556=ORIENTED_EDGE('',*,*,#1932,.T.);
#2557=ORIENTED_EDGE('',*,*,#1931,.T.);
#2558=ORIENTED_EDGE('',*,*,#1933,.F.);
#2559=ORIENTED_EDGE('',*,*,#1923,.F.);
#2560=ORIENTED_EDGE('',*,*,#1933,.T.);
#2561=ORIENTED_EDGE('',*,*,#1930,.T.);
#2562=ORIENTED_EDGE('',*,*,#1927,.T.);
#2563=ORIENTED_EDGE('',*,*,#1924,.T.);
#2564=ORIENTED_EDGE('',*,*,#1932,.F.);
#2565=ORIENTED_EDGE('',*,*,#1922,.F.);
#2566=ORIENTED_EDGE('',*,*,#1926,.F.);
#2567=ORIENTED_EDGE('',*,*,#1929,.F.);
#2568=ORIENTED_EDGE('',*,*,#1934,.F.);
#2569=ORIENTED_EDGE('',*,*,#1935,.F.);
#2570=ORIENTED_EDGE('',*,*,#1936,.T.);
#2571=ORIENTED_EDGE('',*,*,#1934,.T.);
#2572=ORIENTED_EDGE('',*,*,#1936,.F.);
#2573=ORIENTED_EDGE('',*,*,#1937,.F.);
#2574=ORIENTED_EDGE('',*,*,#1938,.T.);
#2575=ORIENTED_EDGE('',*,*,#1935,.T.);
#2576=ORIENTED_EDGE('',*,*,#1938,.F.);
#2577=ORIENTED_EDGE('',*,*,#1939,.F.);
#2578=ORIENTED_EDGE('',*,*,#1940,.T.);
#2579=ORIENTED_EDGE('',*,*,#1937,.T.);
#2580=ORIENTED_EDGE('',*,*,#1940,.F.);
#2581=ORIENTED_EDGE('',*,*,#1939,.T.);
#2582=ORIENTED_EDGE('',*,*,#1941,.F.);
#2583=ORIENTED_EDGE('',*,*,#1942,.F.);
#2584=ORIENTED_EDGE('',*,*,#1943,.T.);
#2585=ORIENTED_EDGE('',*,*,#1941,.T.);
#2586=ORIENTED_EDGE('',*,*,#1943,.F.);
#2587=ORIENTED_EDGE('',*,*,#1944,.F.);
#2588=ORIENTED_EDGE('',*,*,#1945,.T.);
#2589=ORIENTED_EDGE('',*,*,#1942,.T.);
#2590=ORIENTED_EDGE('',*,*,#1945,.F.);
#2591=ORIENTED_EDGE('',*,*,#1946,.F.);
#2592=ORIENTED_EDGE('',*,*,#1947,.T.);
#2593=ORIENTED_EDGE('',*,*,#1944,.T.);
#2594=ORIENTED_EDGE('',*,*,#1947,.F.);
#2595=ORIENTED_EDGE('',*,*,#1946,.T.);
#2596=ORIENTED_EDGE('',*,*,#1948,.T.);
#2597=ORIENTED_EDGE('',*,*,#1949,.T.);
#2598=ORIENTED_EDGE('',*,*,#1950,.T.);
#2599=ORIENTED_EDGE('',*,*,#1951,.F.);
#2600=ORIENTED_EDGE('',*,*,#1952,.T.);
#2601=ORIENTED_EDGE('',*,*,#1953,.T.);
#2602=ORIENTED_EDGE('',*,*,#1954,.T.);
#2603=ORIENTED_EDGE('',*,*,#1949,.F.);
#2604=ORIENTED_EDGE('',*,*,#1955,.T.);
#2605=ORIENTED_EDGE('',*,*,#1956,.T.);
#2606=ORIENTED_EDGE('',*,*,#1957,.T.);
#2607=ORIENTED_EDGE('',*,*,#1953,.F.);
#2608=ORIENTED_EDGE('',*,*,#1958,.T.);
#2609=ORIENTED_EDGE('',*,*,#1959,.T.);
#2610=ORIENTED_EDGE('',*,*,#1960,.T.);
#2611=ORIENTED_EDGE('',*,*,#1956,.F.);
#2612=ORIENTED_EDGE('',*,*,#1961,.T.);
#2613=ORIENTED_EDGE('',*,*,#1962,.T.);
#2614=ORIENTED_EDGE('',*,*,#1963,.T.);
#2615=ORIENTED_EDGE('',*,*,#1959,.F.);
#2616=ORIENTED_EDGE('',*,*,#1964,.T.);
#2617=ORIENTED_EDGE('',*,*,#1951,.T.);
#2618=ORIENTED_EDGE('',*,*,#1965,.T.);
#2619=ORIENTED_EDGE('',*,*,#1962,.F.);
#2620=ORIENTED_EDGE('',*,*,#1964,.F.);
#2621=ORIENTED_EDGE('',*,*,#1961,.F.);
#2622=ORIENTED_EDGE('',*,*,#1958,.F.);
#2623=ORIENTED_EDGE('',*,*,#1955,.F.);
#2624=ORIENTED_EDGE('',*,*,#1952,.F.);
#2625=ORIENTED_EDGE('',*,*,#1948,.F.);
#2626=ORIENTED_EDGE('',*,*,#1965,.F.);
#2627=ORIENTED_EDGE('',*,*,#1950,.F.);
#2628=ORIENTED_EDGE('',*,*,#1954,.F.);
#2629=ORIENTED_EDGE('',*,*,#1957,.F.);
#2630=ORIENTED_EDGE('',*,*,#1960,.F.);
#2631=ORIENTED_EDGE('',*,*,#1963,.F.);
#2632=ORIENTED_EDGE('',*,*,#1966,.F.);
#2633=ORIENTED_EDGE('',*,*,#1967,.T.);
#2634=ORIENTED_EDGE('',*,*,#1968,.F.);
#2635=ORIENTED_EDGE('',*,*,#1967,.F.);
#2636=ORIENTED_EDGE('',*,*,#1969,.F.);
#2637=ORIENTED_EDGE('',*,*,#1970,.T.);
#2638=ORIENTED_EDGE('',*,*,#1971,.F.);
#2639=ORIENTED_EDGE('',*,*,#1970,.F.);
#2640=ORIENTED_EDGE('',*,*,#1972,.F.);
#2641=ORIENTED_EDGE('',*,*,#1973,.T.);
#2642=ORIENTED_EDGE('',*,*,#1974,.F.);
#2643=ORIENTED_EDGE('',*,*,#1973,.F.);
#2644=ORIENTED_EDGE('',*,*,#1975,.F.);
#2645=ORIENTED_EDGE('',*,*,#1976,.T.);
#2646=ORIENTED_EDGE('',*,*,#1977,.F.);
#2647=ORIENTED_EDGE('',*,*,#1976,.F.);
#2648=ORIENTED_EDGE('',*,*,#1978,.T.);
#2649=ORIENTED_EDGE('',*,*,#1979,.T.);
#2650=ORIENTED_EDGE('',*,*,#1980,.F.);
#2651=ORIENTED_EDGE('',*,*,#1981,.F.);
#2652=ORIENTED_EDGE('',*,*,#1982,.T.);
#2653=ORIENTED_EDGE('',*,*,#1981,.T.);
#2654=ORIENTED_EDGE('',*,*,#1983,.F.);
#2655=ORIENTED_EDGE('',*,*,#1984,.F.);
#2656=ORIENTED_EDGE('',*,*,#1985,.T.);
#2657=ORIENTED_EDGE('',*,*,#1984,.T.);
#2658=ORIENTED_EDGE('',*,*,#1986,.F.);
#2659=ORIENTED_EDGE('',*,*,#1987,.F.);
#2660=ORIENTED_EDGE('',*,*,#1988,.T.);
#2661=ORIENTED_EDGE('',*,*,#1987,.T.);
#2662=ORIENTED_EDGE('',*,*,#1989,.F.);
#2663=ORIENTED_EDGE('',*,*,#1979,.F.);
#2664=ORIENTED_EDGE('',*,*,#1989,.T.);
#2665=ORIENTED_EDGE('',*,*,#1986,.T.);
#2666=ORIENTED_EDGE('',*,*,#1983,.T.);
#2667=ORIENTED_EDGE('',*,*,#1980,.T.);
#2668=ORIENTED_EDGE('',*,*,#1968,.T.);
#2669=ORIENTED_EDGE('',*,*,#1971,.T.);
#2670=ORIENTED_EDGE('',*,*,#1974,.T.);
#2671=ORIENTED_EDGE('',*,*,#1977,.T.);
#2672=ORIENTED_EDGE('',*,*,#1988,.F.);
#2673=ORIENTED_EDGE('',*,*,#1978,.F.);
#2674=ORIENTED_EDGE('',*,*,#1982,.F.);
#2675=ORIENTED_EDGE('',*,*,#1985,.F.);
#2676=ORIENTED_EDGE('',*,*,#1966,.T.);
#2677=ORIENTED_EDGE('',*,*,#1969,.T.);
#2678=ORIENTED_EDGE('',*,*,#1972,.T.);
#2679=ORIENTED_EDGE('',*,*,#1975,.T.);
#2680=ORIENTED_EDGE('',*,*,#1990,.F.);
#2681=ORIENTED_EDGE('',*,*,#1991,.T.);
#2682=ORIENTED_EDGE('',*,*,#1992,.F.);
#2683=ORIENTED_EDGE('',*,*,#1991,.F.);
#2684=ORIENTED_EDGE('',*,*,#1990,.T.);
#2685=ORIENTED_EDGE('',*,*,#1993,.F.);
#2686=ORIENTED_EDGE('',*,*,#1994,.T.);
#2687=ORIENTED_EDGE('',*,*,#1995,.F.);
#2688=ORIENTED_EDGE('',*,*,#1994,.F.);
#2689=ORIENTED_EDGE('',*,*,#1993,.T.);
#2690=ORIENTED_EDGE('',*,*,#1996,.F.);
#2691=ORIENTED_EDGE('',*,*,#1997,.F.);
#2692=ORIENTED_EDGE('',*,*,#1998,.F.);
#2693=ORIENTED_EDGE('',*,*,#1999,.F.);
#2694=ORIENTED_EDGE('',*,*,#1997,.T.);
#2695=ORIENTED_EDGE('',*,*,#2000,.T.);
#2696=ORIENTED_EDGE('',*,*,#2001,.F.);
#2697=ORIENTED_EDGE('',*,*,#2002,.F.);
#2698=ORIENTED_EDGE('',*,*,#1996,.T.);
#2699=ORIENTED_EDGE('',*,*,#2003,.T.);
#2700=ORIENTED_EDGE('',*,*,#2004,.F.);
#2701=ORIENTED_EDGE('',*,*,#2000,.F.);
#2702=ORIENTED_EDGE('',*,*,#1998,.T.);
#2703=ORIENTED_EDGE('',*,*,#2002,.T.);
#2704=ORIENTED_EDGE('',*,*,#2005,.F.);
#2705=ORIENTED_EDGE('',*,*,#2006,.F.);
#2706=ORIENTED_EDGE('',*,*,#1999,.T.);
#2707=ORIENTED_EDGE('',*,*,#2006,.T.);
#2708=ORIENTED_EDGE('',*,*,#2007,.F.);
#2709=ORIENTED_EDGE('',*,*,#2003,.F.);
#2710=ORIENTED_EDGE('',*,*,#2007,.T.);
#2711=ORIENTED_EDGE('',*,*,#2005,.T.);
#2712=ORIENTED_EDGE('',*,*,#2001,.T.);
#2713=ORIENTED_EDGE('',*,*,#2004,.T.);
#2714=ORIENTED_EDGE('',*,*,#1992,.T.);
#2715=ORIENTED_EDGE('',*,*,#1995,.T.);
#2716=ORIENTED_EDGE('',*,*,#2008,.F.);
#2717=ORIENTED_EDGE('',*,*,#2009,.T.);
#2718=ORIENTED_EDGE('',*,*,#2010,.T.);
#2719=ORIENTED_EDGE('',*,*,#2009,.F.);
#2720=ORIENTED_EDGE('',*,*,#2008,.T.);
#2721=ORIENTED_EDGE('',*,*,#2010,.F.);
#2722=ORIENTED_EDGE('',*,*,#2011,.T.);
#2723=ORIENTED_EDGE('',*,*,#2012,.T.);
#2724=ORIENTED_EDGE('',*,*,#2013,.T.);
#2725=ORIENTED_EDGE('',*,*,#2014,.F.);
#2726=ORIENTED_EDGE('',*,*,#2015,.T.);
#2727=ORIENTED_EDGE('',*,*,#2016,.T.);
#2728=ORIENTED_EDGE('',*,*,#2017,.T.);
#2729=ORIENTED_EDGE('',*,*,#2012,.F.);
#2730=ORIENTED_EDGE('',*,*,#2018,.T.);
#2731=ORIENTED_EDGE('',*,*,#2019,.T.);
#2732=ORIENTED_EDGE('',*,*,#2020,.T.);
#2733=ORIENTED_EDGE('',*,*,#2016,.F.);
#2734=ORIENTED_EDGE('',*,*,#2021,.T.);
#2735=ORIENTED_EDGE('',*,*,#2022,.T.);
#2736=ORIENTED_EDGE('',*,*,#2023,.T.);
#2737=ORIENTED_EDGE('',*,*,#2019,.F.);
#2738=ORIENTED_EDGE('',*,*,#2024,.T.);
#2739=ORIENTED_EDGE('',*,*,#2025,.T.);
#2740=ORIENTED_EDGE('',*,*,#2026,.T.);
#2741=ORIENTED_EDGE('',*,*,#2022,.F.);
#2742=ORIENTED_EDGE('',*,*,#2027,.T.);
#2743=ORIENTED_EDGE('',*,*,#2014,.T.);
#2744=ORIENTED_EDGE('',*,*,#2028,.T.);
#2745=ORIENTED_EDGE('',*,*,#2025,.F.);
#2746=ORIENTED_EDGE('',*,*,#2027,.F.);
#2747=ORIENTED_EDGE('',*,*,#2024,.F.);
#2748=ORIENTED_EDGE('',*,*,#2021,.F.);
#2749=ORIENTED_EDGE('',*,*,#2018,.F.);
#2750=ORIENTED_EDGE('',*,*,#2015,.F.);
#2751=ORIENTED_EDGE('',*,*,#2011,.F.);
#2752=ORIENTED_EDGE('',*,*,#2028,.F.);
#2753=ORIENTED_EDGE('',*,*,#2013,.F.);
#2754=ORIENTED_EDGE('',*,*,#2017,.F.);
#2755=ORIENTED_EDGE('',*,*,#2020,.F.);
#2756=ORIENTED_EDGE('',*,*,#2023,.F.);
#2757=ORIENTED_EDGE('',*,*,#2026,.F.);
#2758=ORIENTED_EDGE('',*,*,#2029,.F.);
#2759=ORIENTED_EDGE('',*,*,#2030,.F.);
#2760=ORIENTED_EDGE('',*,*,#2031,.F.);
#2761=ORIENTED_EDGE('',*,*,#2032,.T.);
#2762=ORIENTED_EDGE('',*,*,#2030,.T.);
#2763=ORIENTED_EDGE('',*,*,#2032,.F.);
#2764=ORIENTED_EDGE('',*,*,#2033,.F.);
#2765=ORIENTED_EDGE('',*,*,#2034,.T.);
#2766=ORIENTED_EDGE('',*,*,#2031,.T.);
#2767=ORIENTED_EDGE('',*,*,#2034,.F.);
#2768=ORIENTED_EDGE('',*,*,#2035,.F.);
#2769=ORIENTED_EDGE('',*,*,#2036,.T.);
#2770=ORIENTED_EDGE('',*,*,#2033,.T.);
#2771=ORIENTED_EDGE('',*,*,#2036,.F.);
#2772=ORIENTED_EDGE('',*,*,#2035,.T.);
#2773=ORIENTED_EDGE('',*,*,#2037,.F.);
#2774=ORIENTED_EDGE('',*,*,#2038,.F.);
#2775=ORIENTED_EDGE('',*,*,#2039,.T.);
#2776=ORIENTED_EDGE('',*,*,#2037,.T.);
#2777=ORIENTED_EDGE('',*,*,#2039,.F.);
#2778=ORIENTED_EDGE('',*,*,#2029,.T.);
#2779=ORIENTED_EDGE('',*,*,#2040,.T.);
#2780=ORIENTED_EDGE('',*,*,#2038,.T.);
#2781=ORIENTED_EDGE('',*,*,#2040,.F.);
#2782=ORIENTED_EDGE('',*,*,#2041,.F.);
#2783=ORIENTED_EDGE('',*,*,#2042,.T.);
#2784=ORIENTED_EDGE('',*,*,#2043,.T.);
#2785=ORIENTED_EDGE('',*,*,#2042,.F.);
#2786=ORIENTED_EDGE('',*,*,#2041,.T.);
#2787=ORIENTED_EDGE('',*,*,#2043,.F.);
#2788=ORIENTED_EDGE('',*,*,#2044,.F.);
#2789=ORIENTED_EDGE('',*,*,#2045,.T.);
#2790=ORIENTED_EDGE('',*,*,#2046,.T.);
#2791=ORIENTED_EDGE('',*,*,#2045,.F.);
#2792=ORIENTED_EDGE('',*,*,#2047,.F.);
#2793=ORIENTED_EDGE('',*,*,#2048,.T.);
#2794=ORIENTED_EDGE('',*,*,#2049,.T.);
#2795=ORIENTED_EDGE('',*,*,#2048,.F.);
#2796=ORIENTED_EDGE('',*,*,#2047,.T.);
#2797=ORIENTED_EDGE('',*,*,#2044,.T.);
#2798=ORIENTED_EDGE('',*,*,#2049,.F.);
#2799=ORIENTED_EDGE('',*,*,#2046,.F.);
#2800=ORIENTED_EDGE('',*,*,#2050,.F.);
#2801=ORIENTED_EDGE('',*,*,#2051,.F.);
#2802=ORIENTED_EDGE('',*,*,#2052,.T.);
#2803=ORIENTED_EDGE('',*,*,#2053,.F.);
#2804=ORIENTED_EDGE('',*,*,#2052,.F.);
#2805=ORIENTED_EDGE('',*,*,#2054,.F.);
#2806=ORIENTED_EDGE('',*,*,#2055,.F.);
#2807=ORIENTED_EDGE('',*,*,#2056,.F.);
#2808=ORIENTED_EDGE('',*,*,#2057,.F.);
#2809=ORIENTED_EDGE('',*,*,#2058,.F.);
#2810=ORIENTED_EDGE('',*,*,#2059,.T.);
#2811=ORIENTED_EDGE('',*,*,#2060,.F.);
#2812=ORIENTED_EDGE('',*,*,#2061,.F.);
#2813=ORIENTED_EDGE('',*,*,#2062,.F.);
#2814=ORIENTED_EDGE('',*,*,#2063,.F.);
#2815=ORIENTED_EDGE('',*,*,#2064,.F.);
#2816=ORIENTED_EDGE('',*,*,#2065,.F.);
#2817=ORIENTED_EDGE('',*,*,#2059,.F.);
#2818=ORIENTED_EDGE('',*,*,#2055,.T.);
#2819=ORIENTED_EDGE('',*,*,#2066,.T.);
#2820=ORIENTED_EDGE('',*,*,#2064,.T.);
#2821=ORIENTED_EDGE('',*,*,#2067,.F.);
#2822=ORIENTED_EDGE('',*,*,#2054,.T.);
#2823=ORIENTED_EDGE('',*,*,#2068,.T.);
#2824=ORIENTED_EDGE('',*,*,#2065,.T.);
#2825=ORIENTED_EDGE('',*,*,#2066,.F.);
#2826=ORIENTED_EDGE('',*,*,#2051,.T.);
#2827=ORIENTED_EDGE('',*,*,#2069,.T.);
#2828=ORIENTED_EDGE('',*,*,#2060,.T.);
#2829=ORIENTED_EDGE('',*,*,#2068,.F.);
#2830=ORIENTED_EDGE('',*,*,#2070,.F.);
#2831=ORIENTED_EDGE('',*,*,#2071,.T.);
#2832=ORIENTED_EDGE('',*,*,#2072,.T.);
#2833=ORIENTED_EDGE('',*,*,#2071,.F.);
#2834=ORIENTED_EDGE('',*,*,#2050,.T.);
#2835=ORIENTED_EDGE('',*,*,#2073,.T.);
#2836=ORIENTED_EDGE('',*,*,#2061,.T.);
#2837=ORIENTED_EDGE('',*,*,#2069,.F.);
#2838=ORIENTED_EDGE('',*,*,#2056,.T.);
#2839=ORIENTED_EDGE('',*,*,#2067,.T.);
#2840=ORIENTED_EDGE('',*,*,#2063,.T.);
#2841=ORIENTED_EDGE('',*,*,#2074,.F.);
#2842=ORIENTED_EDGE('',*,*,#2057,.T.);
#2843=ORIENTED_EDGE('',*,*,#2074,.T.);
#2844=ORIENTED_EDGE('',*,*,#2062,.T.);
#2845=ORIENTED_EDGE('',*,*,#2073,.F.);
#2846=ORIENTED_EDGE('',*,*,#2058,.T.);
#2847=ORIENTED_EDGE('',*,*,#2070,.T.);
#2848=ORIENTED_EDGE('',*,*,#2053,.T.);
#2849=ORIENTED_EDGE('',*,*,#2072,.F.);
#2850=ORIENTED_EDGE('',*,*,#2075,.F.);
#2851=ORIENTED_EDGE('',*,*,#2076,.F.);
#2852=ORIENTED_EDGE('',*,*,#2077,.F.);
#2853=ORIENTED_EDGE('',*,*,#2078,.F.);
#2854=ORIENTED_EDGE('',*,*,#2079,.F.);
#2855=ORIENTED_EDGE('',*,*,#2080,.F.);
#2856=ORIENTED_EDGE('',*,*,#2081,.F.);
#2857=ORIENTED_EDGE('',*,*,#2082,.F.);
#2858=ORIENTED_EDGE('',*,*,#2083,.F.);
#2859=ORIENTED_EDGE('',*,*,#2084,.F.);
#2860=ORIENTED_EDGE('',*,*,#2085,.F.);
#2861=ORIENTED_EDGE('',*,*,#2086,.F.);
#2862=ORIENTED_EDGE('',*,*,#2087,.F.);
#2863=ORIENTED_EDGE('',*,*,#2088,.F.);
#2864=ORIENTED_EDGE('',*,*,#2089,.F.);
#2865=ORIENTED_EDGE('',*,*,#2090,.F.);
#2866=ORIENTED_EDGE('',*,*,#2091,.F.);
#2867=ORIENTED_EDGE('',*,*,#2092,.F.);
#2868=ORIENTED_EDGE('',*,*,#2093,.F.);
#2869=ORIENTED_EDGE('',*,*,#2094,.F.);
#2870=ORIENTED_EDGE('',*,*,#2095,.F.);
#2871=ORIENTED_EDGE('',*,*,#2096,.F.);
#2872=ORIENTED_EDGE('',*,*,#2097,.F.);
#2873=ORIENTED_EDGE('',*,*,#2098,.F.);
#2874=ORIENTED_EDGE('',*,*,#2076,.T.);
#2875=ORIENTED_EDGE('',*,*,#2099,.T.);
#2876=ORIENTED_EDGE('',*,*,#2096,.T.);
#2877=ORIENTED_EDGE('',*,*,#2100,.T.);
#2878=ORIENTED_EDGE('',*,*,#2082,.T.);
#2879=ORIENTED_EDGE('',*,*,#2101,.T.);
#2880=ORIENTED_EDGE('',*,*,#2084,.T.);
#2881=ORIENTED_EDGE('',*,*,#2102,.T.);
#2882=ORIENTED_EDGE('',*,*,#2088,.T.);
#2883=ORIENTED_EDGE('',*,*,#2103,.T.);
#2884=ORIENTED_EDGE('',*,*,#2092,.T.);
#2885=ORIENTED_EDGE('',*,*,#2104,.T.);
#2886=ORIENTED_EDGE('',*,*,#2105,.T.);
#2887=ORIENTED_EDGE('',*,*,#2087,.T.);
#2888=ORIENTED_EDGE('',*,*,#2106,.T.);
#2889=ORIENTED_EDGE('',*,*,#2093,.T.);
#2890=ORIENTED_EDGE('',*,*,#2103,.F.);
#2891=ORIENTED_EDGE('',*,*,#2083,.T.);
#2892=ORIENTED_EDGE('',*,*,#2107,.T.);
#2893=ORIENTED_EDGE('',*,*,#2089,.T.);
#2894=ORIENTED_EDGE('',*,*,#2102,.F.);
#2895=ORIENTED_EDGE('',*,*,#2079,.T.);
#2896=ORIENTED_EDGE('',*,*,#2100,.F.);
#2897=ORIENTED_EDGE('',*,*,#2095,.T.);
#2898=ORIENTED_EDGE('',*,*,#2108,.T.);
#2899=ORIENTED_EDGE('',*,*,#2081,.T.);
#2900=ORIENTED_EDGE('',*,*,#2109,.T.);
#2901=ORIENTED_EDGE('',*,*,#2085,.T.);
#2902=ORIENTED_EDGE('',*,*,#2101,.F.);
#2903=ORIENTED_EDGE('',*,*,#2075,.T.);
#2904=ORIENTED_EDGE('',*,*,#2110,.T.);
#2905=ORIENTED_EDGE('',*,*,#2097,.T.);
#2906=ORIENTED_EDGE('',*,*,#2099,.F.);
#2907=ORIENTED_EDGE('',*,*,#2077,.T.);
#2908=ORIENTED_EDGE('',*,*,#2104,.F.);
#2909=ORIENTED_EDGE('',*,*,#2091,.T.);
#2910=ORIENTED_EDGE('',*,*,#2111,.T.);
#2911=ORIENTED_EDGE('',*,*,#2112,.F.);
#2912=ORIENTED_EDGE('',*,*,#2113,.T.);
#2913=ORIENTED_EDGE('',*,*,#2114,.T.);
#2914=ORIENTED_EDGE('',*,*,#2115,.F.);
#2915=ORIENTED_EDGE('',*,*,#2116,.F.);
#2916=ORIENTED_EDGE('',*,*,#2115,.T.);
#2917=ORIENTED_EDGE('',*,*,#2117,.T.);
#2918=ORIENTED_EDGE('',*,*,#2118,.F.);
#2919=ORIENTED_EDGE('',*,*,#2119,.F.);
#2920=ORIENTED_EDGE('',*,*,#2118,.T.);
#2921=ORIENTED_EDGE('',*,*,#2120,.T.);
#2922=ORIENTED_EDGE('',*,*,#2121,.F.);
#2923=ORIENTED_EDGE('',*,*,#2122,.F.);
#2924=ORIENTED_EDGE('',*,*,#2121,.T.);
#2925=ORIENTED_EDGE('',*,*,#2123,.T.);
#2926=ORIENTED_EDGE('',*,*,#2124,.F.);
#2927=ORIENTED_EDGE('',*,*,#2125,.F.);
#2928=ORIENTED_EDGE('',*,*,#2126,.T.);
#2929=ORIENTED_EDGE('',*,*,#2127,.T.);
#2930=ORIENTED_EDGE('',*,*,#2113,.F.);
#2931=ORIENTED_EDGE('',*,*,#2128,.F.);
#2932=ORIENTED_EDGE('',*,*,#2124,.T.);
#2933=ORIENTED_EDGE('',*,*,#2129,.T.);
#2934=ORIENTED_EDGE('',*,*,#2126,.F.);
#2935=ORIENTED_EDGE('',*,*,#2129,.F.);
#2936=ORIENTED_EDGE('',*,*,#2123,.F.);
#2937=ORIENTED_EDGE('',*,*,#2120,.F.);
#2938=ORIENTED_EDGE('',*,*,#2117,.F.);
#2939=ORIENTED_EDGE('',*,*,#2114,.F.);
#2940=ORIENTED_EDGE('',*,*,#2127,.F.);
#2941=ORIENTED_EDGE('',*,*,#2130,.F.);
#2942=ORIENTED_EDGE('',*,*,#2105,.F.);
#2943=ORIENTED_EDGE('',*,*,#2131,.T.);
#2944=ORIENTED_EDGE('',*,*,#2130,.T.);
#2945=ORIENTED_EDGE('',*,*,#2131,.F.);
#2946=ORIENTED_EDGE('',*,*,#2078,.T.);
#2947=ORIENTED_EDGE('',*,*,#2111,.F.);
#2948=ORIENTED_EDGE('',*,*,#2094,.T.);
#2949=ORIENTED_EDGE('',*,*,#2106,.F.);
#2950=ORIENTED_EDGE('',*,*,#2090,.T.);
#2951=ORIENTED_EDGE('',*,*,#2107,.F.);
#2952=ORIENTED_EDGE('',*,*,#2086,.T.);
#2953=ORIENTED_EDGE('',*,*,#2109,.F.);
#2954=ORIENTED_EDGE('',*,*,#2080,.T.);
#2955=ORIENTED_EDGE('',*,*,#2108,.F.);
#2956=ORIENTED_EDGE('',*,*,#2098,.T.);
#2957=ORIENTED_EDGE('',*,*,#2110,.F.);
#2958=ORIENTED_EDGE('',*,*,#2122,.T.);
#2959=ORIENTED_EDGE('',*,*,#2128,.T.);
#2960=ORIENTED_EDGE('',*,*,#2125,.T.);
#2961=ORIENTED_EDGE('',*,*,#2112,.T.);
#2962=ORIENTED_EDGE('',*,*,#2116,.T.);
#2963=ORIENTED_EDGE('',*,*,#2119,.T.);
#2964=PLANE('',#3412);
#2965=PLANE('',#3413);
#2966=PLANE('',#3414);
#2967=PLANE('',#3415);
#2968=PLANE('',#3416);
#2969=PLANE('',#3417);
#2970=PLANE('',#3418);
#2971=PLANE('',#3419);
#2972=PLANE('',#3420);
#2973=PLANE('',#3421);
#2974=PLANE('',#3497);
#2975=PLANE('',#3498);
#2976=PLANE('',#3499);
#2977=PLANE('',#3500);
#2978=PLANE('',#3501);
#2979=PLANE('',#3502);
#2980=PLANE('',#3504);
#2981=PLANE('',#3505);
#2982=PLANE('',#3506);
#2983=PLANE('',#3507);
#2984=PLANE('',#3508);
#2985=PLANE('',#3509);
#2986=PLANE('',#3510);
#2987=PLANE('',#3511);
#2988=PLANE('',#3512);
#2989=PLANE('',#3513);
#2990=PLANE('',#3522);
#2991=PLANE('',#3523);
#2992=PLANE('',#3524);
#2993=PLANE('',#3525);
#2994=PLANE('',#3526);
#2995=PLANE('',#3530);
#2996=PLANE('',#3536);
#2997=PLANE('',#3538);
#2998=PLANE('',#3539);
#2999=PLANE('',#3540);
#3000=PLANE('',#3541);
#3001=PLANE('',#3546);
#3002=PLANE('',#3547);
#3003=PLANE('',#3548);
#3004=PLANE('',#3549);
#3005=PLANE('',#3550);
#3006=PLANE('',#3551);
#3007=PLANE('',#3552);
#3008=PLANE('',#3553);
#3009=PLANE('',#3554);
#3010=PLANE('',#3555);
#3011=PLANE('',#3556);
#3012=PLANE('',#3557);
#3013=PLANE('',#3558);
#3014=PLANE('',#3559);
#3015=PLANE('',#3560);
#3016=PLANE('',#3561);
#3017=PLANE('',#3562);
#3018=PLANE('',#3563);
#3019=PLANE('',#3564);
#3020=PLANE('',#3566);
#3021=PLANE('',#3574);
#3022=PLANE('',#3582);
#3023=PLANE('',#3583);
#3024=PLANE('',#3584);
#3025=PLANE('',#3585);
#3026=PLANE('',#3586);
#3027=PLANE('',#3587);
#3028=PLANE('',#3588);
#3029=PLANE('',#3589);
#3030=PLANE('',#3590);
#3031=PLANE('',#3604);
#3032=PLANE('',#3605);
#3033=PLANE('',#3606);
#3034=PLANE('',#3607);
#3035=PLANE('',#3608);
#3036=PLANE('',#3609);
#3037=PLANE('',#3614);
#3038=PLANE('',#3618);
#3039=PLANE('',#3622);
#3040=PLANE('',#3623);
#3041=PLANE('',#3624);
#3042=PLANE('',#3625);
#3043=PLANE('',#3626);
#3044=PLANE('',#3631);
#3045=PLANE('',#3632);
#3046=PLANE('',#3634);
#3047=PLANE('',#3635);
#3048=PLANE('',#3636);
#3049=PLANE('',#3637);
#3050=PLANE('',#3638);
#3051=PLANE('',#3639);
#3052=PLANE('',#3640);
#3053=PLANE('',#3641);
#3054=PLANE('',#3642);
#3055=PLANE('',#3644);
#3056=PLANE('',#3652);
#3057=PLANE('',#3661);
#3058=PLANE('',#3662);
#3059=PLANE('',#3670);
#3060=PLANE('',#3671);
#3061=PLANE('',#3677);
#3062=PLANE('',#3678);
#3063=PLANE('',#3679);
#3064=PLANE('',#3683);
#3065=PLANE('',#3684);
#3066=PLANE('',#3685);
#3067=PLANE('',#3686);
#3068=PLANE('',#3687);
#3069=PLANE('',#3707);
#3070=PLANE('',#3727);
#3071=PLANE('',#3728);
#3072=PLANE('',#3729);
#3073=PLANE('',#3730);
#3074=PLANE('',#3731);
#3075=PLANE('',#3732);
#3076=PLANE('',#3733);
#3077=PLANE('',#3736);
#3078=ADVANCED_FACE('',(#457),#2964,.F.);
#3079=ADVANCED_FACE('',(#458),#2965,.F.);
#3080=ADVANCED_FACE('',(#459),#2966,.F.);
#3081=ADVANCED_FACE('',(#460),#2967,.F.);
#3082=ADVANCED_FACE('',(#461),#2968,.T.);
#3083=ADVANCED_FACE('',(#462),#2969,.F.);
#3084=ADVANCED_FACE('',(#463),#2970,.F.);
#3085=ADVANCED_FACE('',(#464),#2971,.F.);
#3086=ADVANCED_FACE('',(#465),#2972,.F.);
#3087=ADVANCED_FACE('',(#466),#2973,.T.);
#3088=ADVANCED_FACE('',(#467),#397,.F.);
#3089=ADVANCED_FACE('',(#468),#398,.F.);
#3090=ADVANCED_FACE('',(#469),#399,.F.);
#3091=ADVANCED_FACE('',(#470),#400,.F.);
#3092=ADVANCED_FACE('',(#471),#401,.F.);
#3093=ADVANCED_FACE('',(#472),#402,.F.);
#3094=ADVANCED_FACE('',(#473),#403,.F.);
#3095=ADVANCED_FACE('',(#474),#404,.F.);
#3096=ADVANCED_FACE('',(#475),#405,.F.);
#3097=ADVANCED_FACE('',(#476),#406,.F.);
#3098=ADVANCED_FACE('',(#477),#407,.F.);
#3099=ADVANCED_FACE('',(#478),#408,.F.);
#3100=ADVANCED_FACE('',(#479),#409,.F.);
#3101=ADVANCED_FACE('',(#480),#410,.F.);
#3102=ADVANCED_FACE('',(#481),#411,.F.);
#3103=ADVANCED_FACE('',(#482),#412,.F.);
#3104=ADVANCED_FACE('',(#483),#413,.F.);
#3105=ADVANCED_FACE('',(#484),#414,.F.);
#3106=ADVANCED_FACE('',(#485),#415,.F.);
#3107=ADVANCED_FACE('',(#486),#416,.F.);
#3108=ADVANCED_FACE('',(#487),#417,.F.);
#3109=ADVANCED_FACE('',(#488),#418,.F.);
#3110=ADVANCED_FACE('',(#489),#419,.F.);
#3111=ADVANCED_FACE('',(#490),#420,.F.);
#3112=ADVANCED_FACE('',(#491),#421,.F.);
#3113=ADVANCED_FACE('',(#492),#2974,.T.);
#3114=ADVANCED_FACE('',(#493),#2975,.T.);
#3115=ADVANCED_FACE('',(#494),#2976,.T.);
#3116=ADVANCED_FACE('',(#495),#2977,.T.);
#3117=ADVANCED_FACE('',(#496,#192,#193,#194,#195,#196,#197,#198,#199,#200,
#201,#202,#203,#204,#205,#206,#207,#208,#209,#210,#211,#212,#213,#214,#215,
#216,#217,#218),#2978,.T.);
#3118=ADVANCED_FACE('',(#497,#219,#220,#221,#222,#223,#224,#225,#226,#227,
#228,#229,#230,#231,#232,#233,#234,#235,#236,#237,#238,#239,#240,#241,#242,
#243),#2979,.F.);
#3119=ADVANCED_FACE('',(#498),#2980,.F.);
#3120=ADVANCED_FACE('',(#499),#2981,.T.);
#3121=ADVANCED_FACE('',(#500),#2982,.T.);
#3122=ADVANCED_FACE('',(#501),#2983,.T.);
#3123=ADVANCED_FACE('',(#502),#2984,.T.);
#3124=ADVANCED_FACE('',(#503),#2985,.T.);
#3125=ADVANCED_FACE('',(#504),#2986,.F.);
#3126=ADVANCED_FACE('',(#505),#2987,.T.);
#3127=ADVANCED_FACE('',(#506),#2988,.T.);
#3128=ADVANCED_FACE('',(#507),#2989,.T.);
#3129=ADVANCED_FACE('',(#508),#422,.F.);
#3130=ADVANCED_FACE('',(#509),#423,.F.);
#3131=ADVANCED_FACE('',(#510),#2990,.F.);
#3132=ADVANCED_FACE('',(#511),#2991,.F.);
#3133=ADVANCED_FACE('',(#512),#2992,.F.);
#3134=ADVANCED_FACE('',(#513),#2993,.F.);
#3135=ADVANCED_FACE('',(#514),#2994,.F.);
#3136=ADVANCED_FACE('',(#515),#424,.F.);
#3137=ADVANCED_FACE('',(#516,#244),#2995,.T.);
#3138=ADVANCED_FACE('',(#517),#425,.F.);
#3139=ADVANCED_FACE('',(#518,#245),#2996,.T.);
#3140=ADVANCED_FACE('',(#519),#2997,.F.);
#3141=ADVANCED_FACE('',(#520),#2998,.T.);
#3142=ADVANCED_FACE('',(#521),#2999,.F.);
#3143=ADVANCED_FACE('',(#522),#3000,.T.);
#3144=ADVANCED_FACE('',(#523),#426,.F.);
#3145=ADVANCED_FACE('',(#524),#427,.F.);
#3146=ADVANCED_FACE('',(#525),#3001,.T.);
#3147=ADVANCED_FACE('',(#526),#3002,.T.);
#3148=ADVANCED_FACE('',(#527),#3003,.T.);
#3149=ADVANCED_FACE('',(#528),#3004,.T.);
#3150=ADVANCED_FACE('',(#529),#3005,.T.);
#3151=ADVANCED_FACE('',(#530),#3006,.T.);
#3152=ADVANCED_FACE('',(#531,#246,#247,#248),#3007,.F.);
#3153=ADVANCED_FACE('',(#532),#3008,.T.);
#3154=ADVANCED_FACE('',(#533),#3009,.T.);
#3155=ADVANCED_FACE('',(#534),#3010,.T.);
#3156=ADVANCED_FACE('',(#535),#3011,.T.);
#3157=ADVANCED_FACE('',(#536),#3012,.T.);
#3158=ADVANCED_FACE('',(#537),#3013,.F.);
#3159=ADVANCED_FACE('',(#538),#3014,.T.);
#3160=ADVANCED_FACE('',(#539),#3015,.T.);
#3161=ADVANCED_FACE('',(#540),#3016,.T.);
#3162=ADVANCED_FACE('',(#541),#3017,.T.);
#3163=ADVANCED_FACE('',(#542),#3018,.T.);
#3164=ADVANCED_FACE('',(#543),#3019,.F.);
#3165=ADVANCED_FACE('',(#544),#3020,.T.);
#3166=ADVANCED_FACE('',(#545),#129,.T.);
#3167=ADVANCED_FACE('',(#546),#428,.T.);
#3168=ADVANCED_FACE('',(#547),#130,.T.);
#3169=ADVANCED_FACE('',(#548,#249),#3021,.T.);
#3170=ADVANCED_FACE('',(#549),#131,.T.);
#3171=ADVANCED_FACE('',(#550),#429,.T.);
#3172=ADVANCED_FACE('',(#551),#132,.T.);
#3173=ADVANCED_FACE('',(#552),#3022,.T.);
#3174=ADVANCED_FACE('',(#553),#3023,.F.);
#3175=ADVANCED_FACE('',(#554),#3024,.F.);
#3176=ADVANCED_FACE('',(#555),#3025,.F.);
#3177=ADVANCED_FACE('',(#556),#3026,.F.);
#3178=ADVANCED_FACE('',(#557),#3027,.F.);
#3179=ADVANCED_FACE('',(#558),#3028,.F.);
#3180=ADVANCED_FACE('',(#559),#3029,.F.);
#3181=ADVANCED_FACE('',(#560),#3030,.F.);
#3182=ADVANCED_FACE('',(#561),#430,.F.);
#3183=ADVANCED_FACE('',(#562),#431,.F.);
#3184=ADVANCED_FACE('',(#563),#432,.F.);
#3185=ADVANCED_FACE('',(#564),#433,.F.);
#3186=ADVANCED_FACE('',(#565),#3031,.T.);
#3187=ADVANCED_FACE('',(#566),#3032,.T.);
#3188=ADVANCED_FACE('',(#567),#3033,.T.);
#3189=ADVANCED_FACE('',(#568),#3034,.T.);
#3190=ADVANCED_FACE('',(#569,#250,#251,#252,#253),#3035,.T.);
#3191=ADVANCED_FACE('',(#570,#254,#255,#256,#257),#3036,.F.);
#3192=ADVANCED_FACE('',(#571),#434,.F.);
#3193=ADVANCED_FACE('',(#572),#3037,.T.);
#3194=ADVANCED_FACE('',(#573),#435,.F.);
#3195=ADVANCED_FACE('',(#574),#3038,.T.);
#3196=ADVANCED_FACE('',(#575),#436,.F.);
#3197=ADVANCED_FACE('',(#576),#3039,.T.);
#3198=ADVANCED_FACE('',(#577),#3040,.T.);
#3199=ADVANCED_FACE('',(#578),#3041,.T.);
#3200=ADVANCED_FACE('',(#579),#3042,.T.);
#3201=ADVANCED_FACE('',(#580,#258,#259),#3043,.T.);
#3202=ADVANCED_FACE('',(#581),#437,.T.);
#3203=ADVANCED_FACE('',(#582),#3044,.T.);
#3204=ADVANCED_FACE('',(#583),#3045,.F.);
#3205=ADVANCED_FACE('',(#584),#3046,.F.);
#3206=ADVANCED_FACE('',(#585),#3047,.F.);
#3207=ADVANCED_FACE('',(#586),#3048,.F.);
#3208=ADVANCED_FACE('',(#587),#3049,.F.);
#3209=ADVANCED_FACE('',(#588),#3050,.F.);
#3210=ADVANCED_FACE('',(#589),#3051,.F.);
#3211=ADVANCED_FACE('',(#590),#3052,.F.);
#3212=ADVANCED_FACE('',(#591),#3053,.F.);
#3213=ADVANCED_FACE('',(#592),#3054,.F.);
#3214=ADVANCED_FACE('',(#593),#3055,.T.);
#3215=ADVANCED_FACE('',(#594),#133,.T.);
#3216=ADVANCED_FACE('',(#595),#438,.T.);
#3217=ADVANCED_FACE('',(#596),#134,.T.);
#3218=ADVANCED_FACE('',(#597,#260),#3056,.T.);
#3219=ADVANCED_FACE('',(#598),#135,.T.);
#3220=ADVANCED_FACE('',(#599),#439,.T.);
#3221=ADVANCED_FACE('',(#600),#440,.T.);
#3222=ADVANCED_FACE('',(#601),#3057,.T.);
#3223=ADVANCED_FACE('',(#602),#3058,.F.);
#3224=ADVANCED_FACE('',(#603),#441,.F.);
#3225=ADVANCED_FACE('',(#604),#442,.T.);
#3226=ADVANCED_FACE('',(#605,#261),#3059,.T.);
#3227=ADVANCED_FACE('',(#606,#262),#3060,.F.);
#3228=ADVANCED_FACE('',(#607),#136,.T.);
#3229=ADVANCED_FACE('',(#608),#137,.T.);
#3230=ADVANCED_FACE('',(#609),#3061,.T.);
#3231=ADVANCED_FACE('',(#610),#3062,.T.);
#3232=ADVANCED_FACE('',(#611),#3063,.T.);
#3233=ADVANCED_FACE('',(#612),#443,.F.);
#3234=ADVANCED_FACE('',(#613),#3064,.T.);
#3235=ADVANCED_FACE('',(#614),#3065,.T.);
#3236=ADVANCED_FACE('',(#615),#3066,.T.);
#3237=ADVANCED_FACE('',(#616,#263),#3067,.T.);
#3238=ADVANCED_FACE('',(#617,#264),#3068,.F.);
#3239=ADVANCED_FACE('',(#618),#444,.F.);
#3240=ADVANCED_FACE('',(#619),#445,.F.);
#3241=ADVANCED_FACE('',(#620),#446,.F.);
#3242=ADVANCED_FACE('',(#621),#447,.F.);
#3243=ADVANCED_FACE('',(#622),#448,.F.);
#3244=ADVANCED_FACE('',(#623),#449,.F.);
#3245=ADVANCED_FACE('',(#624,#265),#3069,.T.);
#3246=ADVANCED_FACE('',(#625),#450,.T.);
#3247=ADVANCED_FACE('',(#626),#451,.T.);
#3248=ADVANCED_FACE('',(#627),#452,.T.);
#3249=ADVANCED_FACE('',(#628),#453,.T.);
#3250=ADVANCED_FACE('',(#629),#454,.T.);
#3251=ADVANCED_FACE('',(#630),#455,.T.);
#3252=ADVANCED_FACE('',(#631),#3070,.F.);
#3253=ADVANCED_FACE('',(#632),#3071,.F.);
#3254=ADVANCED_FACE('',(#633),#3072,.F.);
#3255=ADVANCED_FACE('',(#634),#3073,.F.);
#3256=ADVANCED_FACE('',(#635),#3074,.F.);
#3257=ADVANCED_FACE('',(#636),#3075,.F.);
#3258=ADVANCED_FACE('',(#637,#266),#3076,.F.);
#3259=ADVANCED_FACE('',(#638),#456,.F.);
#3260=ADVANCED_FACE('',(#639,#267),#3077,.F.);
#3261=CLOSED_SHELL('',(#3078,#3079,#3080,#3081,#3082,#3083,#3084,#3085,
#3086,#3087,#3088,#3089,#3090,#3091,#3092,#3093,#3094,#3095,#3096,#3097,
#3098,#3099,#3100,#3101,#3102,#3103,#3104,#3105,#3106,#3107,#3108,#3109,
#3110,#3111,#3112,#3113,#3114,#3115,#3116,#3117,#3118));
#3262=CLOSED_SHELL('',(#3119,#3120,#3121,#3122,#3123,#3124,#3125,#3126,
#3127,#3128));
#3263=CLOSED_SHELL('',(#3129,#3130,#3131,#3132,#3133,#3134,#3135,#3136,
#3137,#3138,#3139,#3140,#3141,#3142,#3143,#3144,#3145,#3146,#3147,#3148,
#3149,#3150,#3151,#3152));
#3264=CLOSED_SHELL('',(#3153,#3154,#3155,#3156,#3157,#3158));
#3265=CLOSED_SHELL('',(#3159,#3160,#3161,#3162,#3163,#3164));
#3266=CLOSED_SHELL('',(#3165,#3166,#3167,#3168,#3169,#3170,#3171,#3172,
#3173));
#3267=CLOSED_SHELL('',(#3174,#3175,#3176,#3177,#3178,#3179,#3180,#3181));
#3268=CLOSED_SHELL('',(#3182,#3183,#3184,#3185,#3186,#3187,#3188,#3189,
#3190,#3191));
#3269=CLOSED_SHELL('',(#3192,#3193,#3194,#3195,#3196,#3197,#3198,#3199,
#3200,#3201));
#3270=CLOSED_SHELL('',(#3202,#3203,#3204));
#3271=CLOSED_SHELL('',(#3205,#3206,#3207,#3208,#3209,#3210,#3211,#3212));
#3272=CLOSED_SHELL('',(#3213,#3214,#3215,#3216,#3217,#3218,#3219,#3220));
#3273=CLOSED_SHELL('',(#3221,#3222,#3223));
#3274=CLOSED_SHELL('',(#3224,#3225,#3226,#3227));
#3275=CLOSED_SHELL('',(#3228,#3229,#3230,#3231,#3232,#3233,#3234,#3235,
#3236,#3237,#3238));
#3276=CLOSED_SHELL('',(#3239,#3240,#3241,#3242,#3243,#3244,#3245,#3246,
#3247,#3248,#3249,#3250,#3251,#3252,#3253,#3254,#3255,#3256,#3257,#3258,
#3259,#3260));
#3277=DERIVED_UNIT_ELEMENT(#3301,1.);
#3278=DERIVED_UNIT_ELEMENT(#5704,-3.);
#3279=DERIVED_UNIT_ELEMENT(#3301,1.);
#3280=DERIVED_UNIT_ELEMENT(#5704,-3.);
#3281=DERIVED_UNIT_ELEMENT(#3301,1.);
#3282=DERIVED_UNIT_ELEMENT(#5704,-3.);
#3283=DERIVED_UNIT_ELEMENT(#3301,1.);
#3284=DERIVED_UNIT_ELEMENT(#5704,-3.);
#3285=DERIVED_UNIT_ELEMENT(#3301,1.);
#3286=DERIVED_UNIT_ELEMENT(#5704,-3.);
#3287=DERIVED_UNIT_ELEMENT(#3301,1.);
#3288=DERIVED_UNIT_ELEMENT(#5704,-3.);
#3289=DERIVED_UNIT_ELEMENT(#3301,1.);
#3290=DERIVED_UNIT_ELEMENT(#5704,-3.);
#3291=DERIVED_UNIT_ELEMENT(#3301,1.);
#3292=DERIVED_UNIT_ELEMENT(#5704,-3.);
#3293=DERIVED_UNIT_ELEMENT(#3301,1.);
#3294=DERIVED_UNIT_ELEMENT(#5704,-3.);
#3295=DERIVED_UNIT_ELEMENT(#3301,1.);
#3296=DERIVED_UNIT_ELEMENT(#5704,-3.);
#3297=DERIVED_UNIT_ELEMENT(#3301,1.);
#3298=DERIVED_UNIT_ELEMENT(#5704,-3.);
#3299=DERIVED_UNIT_ELEMENT(#3301,1.);
#3300=DERIVED_UNIT_ELEMENT(#5704,-3.);
#3301=(
MASS_UNIT()
NAMED_UNIT(*)
SI_UNIT(.KILO.,.GRAM.)
);
#3302=DERIVED_UNIT((#3277,#3278));
#3303=DERIVED_UNIT((#3279,#3280));
#3304=DERIVED_UNIT((#3281,#3282));
#3305=DERIVED_UNIT((#3283,#3284));
#3306=DERIVED_UNIT((#3285,#3286));
#3307=DERIVED_UNIT((#3287,#3288));
#3308=DERIVED_UNIT((#3289,#3290));
#3309=DERIVED_UNIT((#3291,#3292));
#3310=DERIVED_UNIT((#3293,#3294));
#3311=DERIVED_UNIT((#3295,#3296));
#3312=DERIVED_UNIT((#3297,#3298));
#3313=DERIVED_UNIT((#3299,#3300));
#3314=MEASURE_REPRESENTATION_ITEM('density measure',
POSITIVE_RATIO_MEASURE(7850.),#3302);
#3315=MEASURE_REPRESENTATION_ITEM('density measure',
POSITIVE_RATIO_MEASURE(7850.),#3303);
#3316=MEASURE_REPRESENTATION_ITEM('density measure',
POSITIVE_RATIO_MEASURE(7850.),#3304);
#3317=MEASURE_REPRESENTATION_ITEM('density measure',
POSITIVE_RATIO_MEASURE(7850.),#3305);
#3318=MEASURE_REPRESENTATION_ITEM('density measure',
POSITIVE_RATIO_MEASURE(7850.),#3306);
#3319=MEASURE_REPRESENTATION_ITEM('density measure',
POSITIVE_RATIO_MEASURE(7850.),#3307);
#3320=MEASURE_REPRESENTATION_ITEM('density measure',
POSITIVE_RATIO_MEASURE(7850.),#3308);
#3321=MEASURE_REPRESENTATION_ITEM('density measure',
POSITIVE_RATIO_MEASURE(7850.),#3309);
#3322=MEASURE_REPRESENTATION_ITEM('density measure',
POSITIVE_RATIO_MEASURE(7850.),#3310);
#3323=MEASURE_REPRESENTATION_ITEM('density measure',
POSITIVE_RATIO_MEASURE(7850.),#3311);
#3324=MEASURE_REPRESENTATION_ITEM('density measure',
POSITIVE_RATIO_MEASURE(7850.),#3312);
#3325=MEASURE_REPRESENTATION_ITEM('density measure',
POSITIVE_RATIO_MEASURE(7850.),#3313);
#3326=PROPERTY_DEFINITION_REPRESENTATION(#3386,#3350);
#3327=PROPERTY_DEFINITION_REPRESENTATION(#3387,#3351);
#3328=PROPERTY_DEFINITION_REPRESENTATION(#3388,#3352);
#3329=PROPERTY_DEFINITION_REPRESENTATION(#3389,#3353);
#3330=PROPERTY_DEFINITION_REPRESENTATION(#3390,#3354);
#3331=PROPERTY_DEFINITION_REPRESENTATION(#3391,#3355);
#3332=PROPERTY_DEFINITION_REPRESENTATION(#3392,#3356);
#3333=PROPERTY_DEFINITION_REPRESENTATION(#3393,#3357);
#3334=PROPERTY_DEFINITION_REPRESENTATION(#3394,#3358);
#3335=PROPERTY_DEFINITION_REPRESENTATION(#3395,#3359);
#3336=PROPERTY_DEFINITION_REPRESENTATION(#3396,#3360);
#3337=PROPERTY_DEFINITION_REPRESENTATION(#3397,#3361);
#3338=PROPERTY_DEFINITION_REPRESENTATION(#3398,#3362);
#3339=PROPERTY_DEFINITION_REPRESENTATION(#3399,#3363);
#3340=PROPERTY_DEFINITION_REPRESENTATION(#3400,#3364);
#3341=PROPERTY_DEFINITION_REPRESENTATION(#3401,#3365);
#3342=PROPERTY_DEFINITION_REPRESENTATION(#3402,#3366);
#3343=PROPERTY_DEFINITION_REPRESENTATION(#3403,#3367);
#3344=PROPERTY_DEFINITION_REPRESENTATION(#3404,#3368);
#3345=PROPERTY_DEFINITION_REPRESENTATION(#3405,#3369);
#3346=PROPERTY_DEFINITION_REPRESENTATION(#3406,#3370);
#3347=PROPERTY_DEFINITION_REPRESENTATION(#3407,#3371);
#3348=PROPERTY_DEFINITION_REPRESENTATION(#3408,#3372);
#3349=PROPERTY_DEFINITION_REPRESENTATION(#3409,#3373);
#3350=REPRESENTATION('material name',(#3374),#5690);
#3351=REPRESENTATION('density',(#3314),#5690);
#3352=REPRESENTATION('material name',(#3375),#5691);
#3353=REPRESENTATION('density',(#3315),#5691);
#3354=REPRESENTATION('material name',(#3376),#5692);
#3355=REPRESENTATION('density',(#3316),#5692);
#3356=REPRESENTATION('material name',(#3377),#5693);
#3357=REPRESENTATION('density',(#3317),#5693);
#3358=REPRESENTATION('material name',(#3378),#5694);
#3359=REPRESENTATION('density',(#3318),#5694);
#3360=REPRESENTATION('material name',(#3379),#5695);
#3361=REPRESENTATION('density',(#3319),#5695);
#3362=REPRESENTATION('material name',(#3380),#5696);
#3363=REPRESENTATION('density',(#3320),#5696);
#3364=REPRESENTATION('material name',(#3381),#5697);
#3365=REPRESENTATION('density',(#3321),#5697);
#3366=REPRESENTATION('material name',(#3382),#5698);
#3367=REPRESENTATION('density',(#3322),#5698);
#3368=REPRESENTATION('material name',(#3383),#5699);
#3369=REPRESENTATION('density',(#3323),#5699);
#3370=REPRESENTATION('material name',(#3384),#5700);
#3371=REPRESENTATION('density',(#3324),#5700);
#3372=REPRESENTATION('material name',(#3385),#5701);
#3373=REPRESENTATION('density',(#3325),#5701);
#3374=DESCRIPTIVE_REPRESENTATION_ITEM('Steel','Steel');
#3375=DESCRIPTIVE_REPRESENTATION_ITEM('Steel','Steel');
#3376=DESCRIPTIVE_REPRESENTATION_ITEM('Steel','Steel');
#3377=DESCRIPTIVE_REPRESENTATION_ITEM('Steel','Steel');
#3378=DESCRIPTIVE_REPRESENTATION_ITEM('Steel','Steel');
#3379=DESCRIPTIVE_REPRESENTATION_ITEM('Steel','Steel');
#3380=DESCRIPTIVE_REPRESENTATION_ITEM('Steel','Steel');
#3381=DESCRIPTIVE_REPRESENTATION_ITEM('Steel','Steel');
#3382=DESCRIPTIVE_REPRESENTATION_ITEM('Steel','Steel');
#3383=DESCRIPTIVE_REPRESENTATION_ITEM('Steel','Steel');
#3384=DESCRIPTIVE_REPRESENTATION_ITEM('Steel','Steel');
#3385=DESCRIPTIVE_REPRESENTATION_ITEM('Steel','Steel');
#3386=PROPERTY_DEFINITION('material property','material name',#5774);
#3387=PROPERTY_DEFINITION('material property','density of part',#5774);
#3388=PROPERTY_DEFINITION('material property','material name',#5775);
#3389=PROPERTY_DEFINITION('material property','density of part',#5775);
#3390=PROPERTY_DEFINITION('material property','material name',#5776);
#3391=PROPERTY_DEFINITION('material property','density of part',#5776);
#3392=PROPERTY_DEFINITION('material property','material name',#5777);
#3393=PROPERTY_DEFINITION('material property','density of part',#5777);
#3394=PROPERTY_DEFINITION('material property','material name',#5778);
#3395=PROPERTY_DEFINITION('material property','density of part',#5778);
#3396=PROPERTY_DEFINITION('material property','material name',#5779);
#3397=PROPERTY_DEFINITION('material property','density of part',#5779);
#3398=PROPERTY_DEFINITION('material property','material name',#5780);
#3399=PROPERTY_DEFINITION('material property','density of part',#5780);
#3400=PROPERTY_DEFINITION('material property','material name',#5781);
#3401=PROPERTY_DEFINITION('material property','density of part',#5781);
#3402=PROPERTY_DEFINITION('material property','material name',#5782);
#3403=PROPERTY_DEFINITION('material property','density of part',#5782);
#3404=PROPERTY_DEFINITION('material property','material name',#5783);
#3405=PROPERTY_DEFINITION('material property','density of part',#5783);
#3406=PROPERTY_DEFINITION('material property','material name',#5784);
#3407=PROPERTY_DEFINITION('material property','density of part',#5784);
#3408=PROPERTY_DEFINITION('material property','material name',#5785);
#3409=PROPERTY_DEFINITION('material property','density of part',#5785);
#3410=AXIS2_PLACEMENT_3D('',#4742,#3763,#3764);
#3411=AXIS2_PLACEMENT_3D('',#4743,#3765,#3766);
#3412=AXIS2_PLACEMENT_3D('',#4744,#3767,#3768);
#3413=AXIS2_PLACEMENT_3D('',#4753,#3773,#3774);
#3414=AXIS2_PLACEMENT_3D('',#4759,#3778,#3779);
#3415=AXIS2_PLACEMENT_3D('',#4765,#3783,#3784);
#3416=AXIS2_PLACEMENT_3D('',#4768,#3787,#3788);
#3417=AXIS2_PLACEMENT_3D('',#4769,#3789,#3790);
#3418=AXIS2_PLACEMENT_3D('',#4778,#3795,#3796);
#3419=AXIS2_PLACEMENT_3D('',#4784,#3800,#3801);
#3420=AXIS2_PLACEMENT_3D('',#4790,#3805,#3806);
#3421=AXIS2_PLACEMENT_3D('',#4793,#3809,#3810);
#3422=AXIS2_PLACEMENT_3D('',#4794,#3811,#3812);
#3423=AXIS2_PLACEMENT_3D('',#4796,#3813,#3814);
#3424=AXIS2_PLACEMENT_3D('',#4799,#3816,#3817);
#3425=AXIS2_PLACEMENT_3D('',#4800,#3818,#3819);
#3426=AXIS2_PLACEMENT_3D('',#4802,#3820,#3821);
#3427=AXIS2_PLACEMENT_3D('',#4805,#3823,#3824);
#3428=AXIS2_PLACEMENT_3D('',#4806,#3825,#3826);
#3429=AXIS2_PLACEMENT_3D('',#4808,#3827,#3828);
#3430=AXIS2_PLACEMENT_3D('',#4811,#3830,#3831);
#3431=AXIS2_PLACEMENT_3D('',#4812,#3832,#3833);
#3432=AXIS2_PLACEMENT_3D('',#4814,#3834,#3835);
#3433=AXIS2_PLACEMENT_3D('',#4817,#3837,#3838);
#3434=AXIS2_PLACEMENT_3D('',#4818,#3839,#3840);
#3435=AXIS2_PLACEMENT_3D('',#4820,#3841,#3842);
#3436=AXIS2_PLACEMENT_3D('',#4823,#3844,#3845);
#3437=AXIS2_PLACEMENT_3D('',#4824,#3846,#3847);
#3438=AXIS2_PLACEMENT_3D('',#4826,#3848,#3849);
#3439=AXIS2_PLACEMENT_3D('',#4829,#3851,#3852);
#3440=AXIS2_PLACEMENT_3D('',#4830,#3853,#3854);
#3441=AXIS2_PLACEMENT_3D('',#4832,#3855,#3856);
#3442=AXIS2_PLACEMENT_3D('',#4835,#3858,#3859);
#3443=AXIS2_PLACEMENT_3D('',#4836,#3860,#3861);
#3444=AXIS2_PLACEMENT_3D('',#4838,#3862,#3863);
#3445=AXIS2_PLACEMENT_3D('',#4841,#3865,#3866);
#3446=AXIS2_PLACEMENT_3D('',#4842,#3867,#3868);
#3447=AXIS2_PLACEMENT_3D('',#4844,#3869,#3870);
#3448=AXIS2_PLACEMENT_3D('',#4847,#3872,#3873);
#3449=AXIS2_PLACEMENT_3D('',#4848,#3874,#3875);
#3450=AXIS2_PLACEMENT_3D('',#4850,#3876,#3877);
#3451=AXIS2_PLACEMENT_3D('',#4853,#3879,#3880);
#3452=AXIS2_PLACEMENT_3D('',#4854,#3881,#3882);
#3453=AXIS2_PLACEMENT_3D('',#4856,#3883,#3884);
#3454=AXIS2_PLACEMENT_3D('',#4859,#3886,#3887);
#3455=AXIS2_PLACEMENT_3D('',#4860,#3888,#3889);
#3456=AXIS2_PLACEMENT_3D('',#4862,#3890,#3891);
#3457=AXIS2_PLACEMENT_3D('',#4865,#3893,#3894);
#3458=AXIS2_PLACEMENT_3D('',#4866,#3895,#3896);
#3459=AXIS2_PLACEMENT_3D('',#4868,#3897,#3898);
#3460=AXIS2_PLACEMENT_3D('',#4871,#3900,#3901);
#3461=AXIS2_PLACEMENT_3D('',#4872,#3902,#3903);
#3462=AXIS2_PLACEMENT_3D('',#4874,#3904,#3905);
#3463=AXIS2_PLACEMENT_3D('',#4877,#3907,#3908);
#3464=AXIS2_PLACEMENT_3D('',#4878,#3909,#3910);
#3465=AXIS2_PLACEMENT_3D('',#4880,#3911,#3912);
#3466=AXIS2_PLACEMENT_3D('',#4883,#3914,#3915);
#3467=AXIS2_PLACEMENT_3D('',#4884,#3916,#3917);
#3468=AXIS2_PLACEMENT_3D('',#4886,#3918,#3919);
#3469=AXIS2_PLACEMENT_3D('',#4889,#3921,#3922);
#3470=AXIS2_PLACEMENT_3D('',#4890,#3923,#3924);
#3471=AXIS2_PLACEMENT_3D('',#4892,#3925,#3926);
#3472=AXIS2_PLACEMENT_3D('',#4895,#3928,#3929);
#3473=AXIS2_PLACEMENT_3D('',#4896,#3930,#3931);
#3474=AXIS2_PLACEMENT_3D('',#4898,#3932,#3933);
#3475=AXIS2_PLACEMENT_3D('',#4901,#3935,#3936);
#3476=AXIS2_PLACEMENT_3D('',#4902,#3937,#3938);
#3477=AXIS2_PLACEMENT_3D('',#4904,#3939,#3940);
#3478=AXIS2_PLACEMENT_3D('',#4907,#3942,#3943);
#3479=AXIS2_PLACEMENT_3D('',#4908,#3944,#3945);
#3480=AXIS2_PLACEMENT_3D('',#4910,#3946,#3947);
#3481=AXIS2_PLACEMENT_3D('',#4913,#3949,#3950);
#3482=AXIS2_PLACEMENT_3D('',#4914,#3951,#3952);
#3483=AXIS2_PLACEMENT_3D('',#4916,#3953,#3954);
#3484=AXIS2_PLACEMENT_3D('',#4919,#3956,#3957);
#3485=AXIS2_PLACEMENT_3D('',#4920,#3958,#3959);
#3486=AXIS2_PLACEMENT_3D('',#4922,#3960,#3961);
#3487=AXIS2_PLACEMENT_3D('',#4925,#3963,#3964);
#3488=AXIS2_PLACEMENT_3D('',#4926,#3965,#3966);
#3489=AXIS2_PLACEMENT_3D('',#4928,#3967,#3968);
#3490=AXIS2_PLACEMENT_3D('',#4931,#3970,#3971);
#3491=AXIS2_PLACEMENT_3D('',#4932,#3972,#3973);
#3492=AXIS2_PLACEMENT_3D('',#4934,#3974,#3975);
#3493=AXIS2_PLACEMENT_3D('',#4937,#3977,#3978);
#3494=AXIS2_PLACEMENT_3D('',#4938,#3979,#3980);
#3495=AXIS2_PLACEMENT_3D('',#4940,#3981,#3982);
#3496=AXIS2_PLACEMENT_3D('',#4943,#3984,#3985);
#3497=AXIS2_PLACEMENT_3D('',#4944,#3986,#3987);
#3498=AXIS2_PLACEMENT_3D('',#4953,#3992,#3993);
#3499=AXIS2_PLACEMENT_3D('',#4959,#3997,#3998);
#3500=AXIS2_PLACEMENT_3D('',#4965,#4002,#4003);
#3501=AXIS2_PLACEMENT_3D('',#4968,#4006,#4007);
#3502=AXIS2_PLACEMENT_3D('',#4969,#4008,#4009);
#3503=AXIS2_PLACEMENT_3D('',#4970,#4010,#4011);
#3504=AXIS2_PLACEMENT_3D('',#4971,#4012,#4013);
#3505=AXIS2_PLACEMENT_3D('',#4988,#4022,#4023);
#3506=AXIS2_PLACEMENT_3D('',#4994,#4027,#4028);
#3507=AXIS2_PLACEMENT_3D('',#4998,#4031,#4032);
#3508=AXIS2_PLACEMENT_3D('',#5002,#4035,#4036);
#3509=AXIS2_PLACEMENT_3D('',#5006,#4039,#4040);
#3510=AXIS2_PLACEMENT_3D('',#5014,#4045,#4046);
#3511=AXIS2_PLACEMENT_3D('',#5016,#4048,#4049);
#3512=AXIS2_PLACEMENT_3D('',#5018,#4051,#4052);
#3513=AXIS2_PLACEMENT_3D('',#5020,#4054,#4055);
#3514=AXIS2_PLACEMENT_3D('',#5021,#4056,#4057);
#3515=AXIS2_PLACEMENT_3D('',#5022,#4058,#4059);
#3516=AXIS2_PLACEMENT_3D('',#5027,#4061,#4062);
#3517=AXIS2_PLACEMENT_3D('',#5030,#4064,#4065);
#3518=AXIS2_PLACEMENT_3D('',#5031,#4066,#4067);
#3519=AXIS2_PLACEMENT_3D('',#5036,#4069,#4070);
#3520=AXIS2_PLACEMENT_3D('',#5040,#4072,#4073);
#3521=AXIS2_PLACEMENT_3D('',#5041,#4074,#4075);
#3522=AXIS2_PLACEMENT_3D('',#5042,#4076,#4077);
#3523=AXIS2_PLACEMENT_3D('',#5051,#4082,#4083);
#3524=AXIS2_PLACEMENT_3D('',#5057,#4087,#4088);
#3525=AXIS2_PLACEMENT_3D('',#5063,#4092,#4093);
#3526=AXIS2_PLACEMENT_3D('',#5066,#4096,#4097);
#3527=AXIS2_PLACEMENT_3D('',#5067,#4098,#4099);
#3528=AXIS2_PLACEMENT_3D('',#5068,#4100,#4101);
#3529=AXIS2_PLACEMENT_3D('',#5070,#4103,#4104);
#3530=AXIS2_PLACEMENT_3D('',#5071,#4105,#4106);
#3531=AXIS2_PLACEMENT_3D('',#5073,#4107,#4108);
#3532=AXIS2_PLACEMENT_3D('',#5074,#4109,#4110);
#3533=AXIS2_PLACEMENT_3D('',#5076,#4111,#4112);
#3534=AXIS2_PLACEMENT_3D('',#5077,#4113,#4114);
#3535=AXIS2_PLACEMENT_3D('',#5079,#4116,#4117);
#3536=AXIS2_PLACEMENT_3D('',#5080,#4118,#4119);
#3537=AXIS2_PLACEMENT_3D('',#5082,#4120,#4121);
#3538=AXIS2_PLACEMENT_3D('',#5083,#4122,#4123);
#3539=AXIS2_PLACEMENT_3D('',#5093,#4129,#4130);
#3540=AXIS2_PLACEMENT_3D('',#5097,#4133,#4134);
#3541=AXIS2_PLACEMENT_3D('',#5104,#4139,#4140);
#3542=AXIS2_PLACEMENT_3D('',#5108,#4143,#4144);
#3543=AXIS2_PLACEMENT_3D('',#5110,#4145,#4146);
#3544=AXIS2_PLACEMENT_3D('',#5112,#4148,#4149);
#3545=AXIS2_PLACEMENT_3D('',#5114,#4150,#4151);
#3546=AXIS2_PLACEMENT_3D('',#5116,#4153,#4154);
#3547=AXIS2_PLACEMENT_3D('',#5120,#4157,#4158);
#3548=AXIS2_PLACEMENT_3D('',#5124,#4161,#4162);
#3549=AXIS2_PLACEMENT_3D('',#5130,#4166,#4167);
#3550=AXIS2_PLACEMENT_3D('',#5134,#4170,#4171);
#3551=AXIS2_PLACEMENT_3D('',#5138,#4174,#4175);
#3552=AXIS2_PLACEMENT_3D('',#5140,#4177,#4178);
#3553=AXIS2_PLACEMENT_3D('',#5141,#4179,#4180);
#3554=AXIS2_PLACEMENT_3D('',#5150,#4185,#4186);
#3555=AXIS2_PLACEMENT_3D('',#5156,#4190,#4191);
#3556=AXIS2_PLACEMENT_3D('',#5162,#4195,#4196);
#3557=AXIS2_PLACEMENT_3D('',#5165,#4199,#4200);
#3558=AXIS2_PLACEMENT_3D('',#5166,#4201,#4202);
#3559=AXIS2_PLACEMENT_3D('',#5167,#4203,#4204);
#3560=AXIS2_PLACEMENT_3D('',#5176,#4209,#4210);
#3561=AXIS2_PLACEMENT_3D('',#5182,#4214,#4215);
#3562=AXIS2_PLACEMENT_3D('',#5188,#4219,#4220);
#3563=AXIS2_PLACEMENT_3D('',#5191,#4223,#4224);
#3564=AXIS2_PLACEMENT_3D('',#5192,#4225,#4226);
#3565=AXIS2_PLACEMENT_3D('',#5193,#4227,#4228);
#3566=AXIS2_PLACEMENT_3D('',#5194,#4229,#4230);
#3567=AXIS2_PLACEMENT_3D('',#5196,#4231,#4232);
#3568=AXIS2_PLACEMENT_3D('',#5197,#4233,#4234);
#3569=AXIS2_PLACEMENT_3D('',#5199,#4235,#4236);
#3570=AXIS2_PLACEMENT_3D('',#5201,#4238,#4239);
#3571=AXIS2_PLACEMENT_3D('',#5203,#4240,#4241);
#3572=AXIS2_PLACEMENT_3D('',#5205,#4243,#4244);
#3573=AXIS2_PLACEMENT_3D('',#5207,#4245,#4246);
#3574=AXIS2_PLACEMENT_3D('',#5209,#4248,#4249);
#3575=AXIS2_PLACEMENT_3D('',#5211,#4250,#4251);
#3576=AXIS2_PLACEMENT_3D('',#5212,#4252,#4253);
#3577=AXIS2_PLACEMENT_3D('',#5214,#4254,#4255);
#3578=AXIS2_PLACEMENT_3D('',#5216,#4257,#4258);
#3579=AXIS2_PLACEMENT_3D('',#5218,#4259,#4260);
#3580=AXIS2_PLACEMENT_3D('',#5220,#4262,#4263);
#3581=AXIS2_PLACEMENT_3D('',#5222,#4264,#4265);
#3582=AXIS2_PLACEMENT_3D('',#5224,#4267,#4268);
#3583=AXIS2_PLACEMENT_3D('',#5225,#4269,#4270);
#3584=AXIS2_PLACEMENT_3D('',#5234,#4275,#4276);
#3585=AXIS2_PLACEMENT_3D('',#5240,#4280,#4281);
#3586=AXIS2_PLACEMENT_3D('',#5246,#4285,#4286);
#3587=AXIS2_PLACEMENT_3D('',#5252,#4290,#4291);
#3588=AXIS2_PLACEMENT_3D('',#5258,#4295,#4296);
#3589=AXIS2_PLACEMENT_3D('',#5261,#4299,#4300);
#3590=AXIS2_PLACEMENT_3D('',#5262,#4301,#4302);
#3591=AXIS2_PLACEMENT_3D('',#5263,#4303,#4304);
#3592=AXIS2_PLACEMENT_3D('',#5264,#4305,#4306);
#3593=AXIS2_PLACEMENT_3D('',#5266,#4307,#4308);
#3594=AXIS2_PLACEMENT_3D('',#5269,#4310,#4311);
#3595=AXIS2_PLACEMENT_3D('',#5270,#4312,#4313);
#3596=AXIS2_PLACEMENT_3D('',#5272,#4314,#4315);
#3597=AXIS2_PLACEMENT_3D('',#5275,#4317,#4318);
#3598=AXIS2_PLACEMENT_3D('',#5276,#4319,#4320);
#3599=AXIS2_PLACEMENT_3D('',#5278,#4321,#4322);
#3600=AXIS2_PLACEMENT_3D('',#5281,#4324,#4325);
#3601=AXIS2_PLACEMENT_3D('',#5282,#4326,#4327);
#3602=AXIS2_PLACEMENT_3D('',#5284,#4328,#4329);
#3603=AXIS2_PLACEMENT_3D('',#5287,#4331,#4332);
#3604=AXIS2_PLACEMENT_3D('',#5288,#4333,#4334);
#3605=AXIS2_PLACEMENT_3D('',#5297,#4339,#4340);
#3606=AXIS2_PLACEMENT_3D('',#5303,#4344,#4345);
#3607=AXIS2_PLACEMENT_3D('',#5309,#4349,#4350);
#3608=AXIS2_PLACEMENT_3D('',#5312,#4353,#4354);
#3609=AXIS2_PLACEMENT_3D('',#5313,#4355,#4356);
#3610=AXIS2_PLACEMENT_3D('',#5314,#4357,#4358);
#3611=AXIS2_PLACEMENT_3D('',#5315,#4359,#4360);
#3612=AXIS2_PLACEMENT_3D('',#5317,#4361,#4362);
#3613=AXIS2_PLACEMENT_3D('',#5320,#4364,#4365);
#3614=AXIS2_PLACEMENT_3D('',#5321,#4366,#4367);
#3615=AXIS2_PLACEMENT_3D('',#5322,#4368,#4369);
#3616=AXIS2_PLACEMENT_3D('',#5324,#4370,#4371);
#3617=AXIS2_PLACEMENT_3D('',#5327,#4373,#4374);
#3618=AXIS2_PLACEMENT_3D('',#5328,#4375,#4376);
#3619=AXIS2_PLACEMENT_3D('',#5329,#4377,#4378);
#3620=AXIS2_PLACEMENT_3D('',#5334,#4380,#4381);
#3621=AXIS2_PLACEMENT_3D('',#5337,#4383,#4384);
#3622=AXIS2_PLACEMENT_3D('',#5338,#4385,#4386);
#3623=AXIS2_PLACEMENT_3D('',#5344,#4390,#4391);
#3624=AXIS2_PLACEMENT_3D('',#5348,#4394,#4395);
#3625=AXIS2_PLACEMENT_3D('',#5352,#4398,#4399);
#3626=AXIS2_PLACEMENT_3D('',#5354,#4401,#4402);
#3627=AXIS2_PLACEMENT_3D('',#5355,#4403,#4404);
#3628=AXIS2_PLACEMENT_3D('',#5356,#4405,#4406);
#3629=AXIS2_PLACEMENT_3D('',#5358,#4407,#4408);
#3630=AXIS2_PLACEMENT_3D('',#5361,#4410,#4411);
#3631=AXIS2_PLACEMENT_3D('',#5362,#4412,#4413);
#3632=AXIS2_PLACEMENT_3D('',#5363,#4414,#4415);
#3633=AXIS2_PLACEMENT_3D('',#5364,#4416,#4417);
#3634=AXIS2_PLACEMENT_3D('',#5365,#4418,#4419);
#3635=AXIS2_PLACEMENT_3D('',#5374,#4424,#4425);
#3636=AXIS2_PLACEMENT_3D('',#5380,#4429,#4430);
#3637=AXIS2_PLACEMENT_3D('',#5386,#4434,#4435);
#3638=AXIS2_PLACEMENT_3D('',#5392,#4439,#4440);
#3639=AXIS2_PLACEMENT_3D('',#5398,#4444,#4445);
#3640=AXIS2_PLACEMENT_3D('',#5401,#4448,#4449);
#3641=AXIS2_PLACEMENT_3D('',#5402,#4450,#4451);
#3642=AXIS2_PLACEMENT_3D('',#5403,#4452,#4453);
#3643=AXIS2_PLACEMENT_3D('',#5405,#4454,#4455);
#3644=AXIS2_PLACEMENT_3D('',#5406,#4456,#4457);
#3645=AXIS2_PLACEMENT_3D('',#5408,#4458,#4459);
#3646=AXIS2_PLACEMENT_3D('',#5409,#4460,#4461);
#3647=AXIS2_PLACEMENT_3D('',#5411,#4462,#4463);
#3648=AXIS2_PLACEMENT_3D('',#5413,#4465,#4466);
#3649=AXIS2_PLACEMENT_3D('',#5415,#4467,#4468);
#3650=AXIS2_PLACEMENT_3D('',#5417,#4470,#4471);
#3651=AXIS2_PLACEMENT_3D('',#5419,#4472,#4473);
#3652=AXIS2_PLACEMENT_3D('',#5421,#4475,#4476);
#3653=AXIS2_PLACEMENT_3D('',#5423,#4477,#4478);
#3654=AXIS2_PLACEMENT_3D('',#5424,#4479,#4480);
#3655=AXIS2_PLACEMENT_3D('',#5426,#4481,#4482);
#3656=AXIS2_PLACEMENT_3D('',#5428,#4484,#4485);
#3657=AXIS2_PLACEMENT_3D('',#5430,#4487,#4488);
#3658=AXIS2_PLACEMENT_3D('',#5431,#4489,#4490);
#3659=AXIS2_PLACEMENT_3D('',#5433,#4491,#4492);
#3660=AXIS2_PLACEMENT_3D('',#5436,#4494,#4495);
#3661=AXIS2_PLACEMENT_3D('',#5437,#4496,#4497);
#3662=AXIS2_PLACEMENT_3D('',#5438,#4498,#4499);
#3663=AXIS2_PLACEMENT_3D('',#5439,#4500,#4501);
#3664=AXIS2_PLACEMENT_3D('',#5440,#4502,#4503);
#3665=AXIS2_PLACEMENT_3D('',#5442,#4504,#4505);
#3666=AXIS2_PLACEMENT_3D('',#5445,#4507,#4508);
#3667=AXIS2_PLACEMENT_3D('',#5446,#4509,#4510);
#3668=AXIS2_PLACEMENT_3D('',#5448,#4511,#4512);
#3669=AXIS2_PLACEMENT_3D('',#5451,#4514,#4515);
#3670=AXIS2_PLACEMENT_3D('',#5452,#4516,#4517);
#3671=AXIS2_PLACEMENT_3D('',#5453,#4518,#4519);
#3672=AXIS2_PLACEMENT_3D('',#5454,#4520,#4521);
#3673=AXIS2_PLACEMENT_3D('',#5455,#4522,#4523);
#3674=AXIS2_PLACEMENT_3D('',#5467,#4525,#4526);
#3675=AXIS2_PLACEMENT_3D('',#5483,#4527,#4528);
#3676=AXIS2_PLACEMENT_3D('',#5485,#4529,#4530);
#3677=AXIS2_PLACEMENT_3D('',#5511,#4532,#4533);
#3678=AXIS2_PLACEMENT_3D('',#5514,#4536,#4537);
#3679=AXIS2_PLACEMENT_3D('',#5516,#4539,#4540);
#3680=AXIS2_PLACEMENT_3D('',#5518,#4542,#4543);
#3681=AXIS2_PLACEMENT_3D('',#5520,#4544,#4545);
#3682=AXIS2_PLACEMENT_3D('',#5523,#4547,#4548);
#3683=AXIS2_PLACEMENT_3D('',#5524,#4549,#4550);
#3684=AXIS2_PLACEMENT_3D('',#5526,#4552,#4553);
#3685=AXIS2_PLACEMENT_3D('',#5528,#4555,#4556);
#3686=AXIS2_PLACEMENT_3D('',#5529,#4557,#4558);
#3687=AXIS2_PLACEMENT_3D('',#5530,#4559,#4560);
#3688=AXIS2_PLACEMENT_3D('',#5531,#4561,#4562);
#3689=AXIS2_PLACEMENT_3D('',#5532,#4563,#4564);
#3690=AXIS2_PLACEMENT_3D('',#5537,#4566,#4567);
#3691=AXIS2_PLACEMENT_3D('',#5540,#4569,#4570);
#3692=AXIS2_PLACEMENT_3D('',#5541,#4571,#4572);
#3693=AXIS2_PLACEMENT_3D('',#5546,#4574,#4575);
#3694=AXIS2_PLACEMENT_3D('',#5549,#4577,#4578);
#3695=AXIS2_PLACEMENT_3D('',#5550,#4579,#4580);
#3696=AXIS2_PLACEMENT_3D('',#5555,#4582,#4583);
#3697=AXIS2_PLACEMENT_3D('',#5558,#4585,#4586);
#3698=AXIS2_PLACEMENT_3D('',#5559,#4587,#4588);
#3699=AXIS2_PLACEMENT_3D('',#5564,#4590,#4591);
#3700=AXIS2_PLACEMENT_3D('',#5567,#4593,#4594);
#3701=AXIS2_PLACEMENT_3D('',#5568,#4595,#4596);
#3702=AXIS2_PLACEMENT_3D('',#5573,#4598,#4599);
#3703=AXIS2_PLACEMENT_3D('',#5576,#4601,#4602);
#3704=AXIS2_PLACEMENT_3D('',#5577,#4603,#4604);
#3705=AXIS2_PLACEMENT_3D('',#5582,#4606,#4607);
#3706=AXIS2_PLACEMENT_3D('',#5585,#4609,#4610);
#3707=AXIS2_PLACEMENT_3D('',#5586,#4611,#4612);
#3708=AXIS2_PLACEMENT_3D('',#5587,#4613,#4614);
#3709=AXIS2_PLACEMENT_3D('',#5588,#4615,#4616);
#3710=AXIS2_PLACEMENT_3D('',#5589,#4617,#4618);
#3711=AXIS2_PLACEMENT_3D('',#5590,#4619,#4620);
#3712=AXIS2_PLACEMENT_3D('',#5591,#4621,#4622);
#3713=AXIS2_PLACEMENT_3D('',#5592,#4623,#4624);
#3714=AXIS2_PLACEMENT_3D('',#5594,#4625,#4626);
#3715=AXIS2_PLACEMENT_3D('',#5595,#4627,#4628);
#3716=AXIS2_PLACEMENT_3D('',#5596,#4629,#4630);
#3717=AXIS2_PLACEMENT_3D('',#5597,#4631,#4632);
#3718=AXIS2_PLACEMENT_3D('',#5598,#4633,#4634);
#3719=AXIS2_PLACEMENT_3D('',#5599,#4635,#4636);
#3720=AXIS2_PLACEMENT_3D('',#5600,#4637,#4638);
#3721=AXIS2_PLACEMENT_3D('',#5601,#4639,#4640);
#3722=AXIS2_PLACEMENT_3D('',#5602,#4641,#4642);
#3723=AXIS2_PLACEMENT_3D('',#5603,#4643,#4644);
#3724=AXIS2_PLACEMENT_3D('',#5604,#4645,#4646);
#3725=AXIS2_PLACEMENT_3D('',#5605,#4647,#4648);
#3726=AXIS2_PLACEMENT_3D('',#5606,#4649,#4650);
#3727=AXIS2_PLACEMENT_3D('',#5607,#4651,#4652);
#3728=AXIS2_PLACEMENT_3D('',#5616,#4657,#4658);
#3729=AXIS2_PLACEMENT_3D('',#5622,#4662,#4663);
#3730=AXIS2_PLACEMENT_3D('',#5628,#4667,#4668);
#3731=AXIS2_PLACEMENT_3D('',#5634,#4672,#4673);
#3732=AXIS2_PLACEMENT_3D('',#5640,#4677,#4678);
#3733=AXIS2_PLACEMENT_3D('',#5643,#4681,#4682);
#3734=AXIS2_PLACEMENT_3D('',#5645,#4683,#4684);
#3735=AXIS2_PLACEMENT_3D('',#5646,#4685,#4686);
#3736=AXIS2_PLACEMENT_3D('',#5648,#4688,#4689);
#3737=AXIS2_PLACEMENT_3D('',#5649,#4690,#4691);
#3738=AXIS2_PLACEMENT_3D('',#5650,#4692,#4693);
#3739=AXIS2_PLACEMENT_3D('',#5651,#4694,#4695);
#3740=AXIS2_PLACEMENT_3D('',#5652,#4696,#4697);
#3741=AXIS2_PLACEMENT_3D('',#5653,#4698,#4699);
#3742=AXIS2_PLACEMENT_3D('',#5654,#4700,#4701);
#3743=AXIS2_PLACEMENT_3D('',#5655,#4702,#4703);
#3744=AXIS2_PLACEMENT_3D('',#5656,#4704,#4705);
#3745=AXIS2_PLACEMENT_3D('',#5657,#4706,#4707);
#3746=AXIS2_PLACEMENT_3D('',#5658,#4708,#4709);
#3747=AXIS2_PLACEMENT_3D('',#5659,#4710,#4711);
#3748=AXIS2_PLACEMENT_3D('',#5660,#4712,#4713);
#3749=AXIS2_PLACEMENT_3D('',#5661,#4714,#4715);
#3750=AXIS2_PLACEMENT_3D('',#5662,#4716,#4717);
#3751=AXIS2_PLACEMENT_3D('',#5663,#4718,#4719);
#3752=AXIS2_PLACEMENT_3D('',#5664,#4720,#4721);
#3753=AXIS2_PLACEMENT_3D('',#5665,#4722,#4723);
#3754=AXIS2_PLACEMENT_3D('',#5666,#4724,#4725);
#3755=AXIS2_PLACEMENT_3D('',#5667,#4726,#4727);
#3756=AXIS2_PLACEMENT_3D('',#5668,#4728,#4729);
#3757=AXIS2_PLACEMENT_3D('',#5669,#4730,#4731);
#3758=AXIS2_PLACEMENT_3D('',#5670,#4732,#4733);
#3759=AXIS2_PLACEMENT_3D('',#5671,#4734,#4735);
#3760=AXIS2_PLACEMENT_3D('',#5672,#4736,#4737);
#3761=AXIS2_PLACEMENT_3D('',#5673,#4738,#4739);
#3762=AXIS2_PLACEMENT_3D('',#5674,#4740,#4741);
#3763=DIRECTION('axis',(0.,0.,1.));
#3764=DIRECTION('refdir',(1.,0.,0.));
#3765=DIRECTION('axis',(0.,0.,1.));
#3766=DIRECTION('refdir',(1.,0.,0.));
#3767=DIRECTION('center_axis',(0.,-1.,0.));
#3768=DIRECTION('ref_axis',(1.,0.,0.));
#3769=DIRECTION('',(-1.,0.,0.));
#3770=DIRECTION('',(0.,0.,1.));
#3771=DIRECTION('',(1.,0.,0.));
#3772=DIRECTION('',(0.,0.,1.));
#3773=DIRECTION('center_axis',(-1.,0.,0.));
#3774=DIRECTION('ref_axis',(0.,-1.,0.));
#3775=DIRECTION('',(0.,1.,0.));
#3776=DIRECTION('',(0.,-1.,0.));
#3777=DIRECTION('',(0.,0.,1.));
#3778=DIRECTION('center_axis',(0.,1.,0.));
#3779=DIRECTION('ref_axis',(-1.,0.,0.));
#3780=DIRECTION('',(1.,0.,0.));
#3781=DIRECTION('',(-1.,0.,0.));
#3782=DIRECTION('',(0.,0.,1.));
#3783=DIRECTION('center_axis',(1.,0.,0.));
#3784=DIRECTION('ref_axis',(0.,1.,0.));
#3785=DIRECTION('',(0.,-1.,0.));
#3786=DIRECTION('',(0.,1.,0.));
#3787=DIRECTION('center_axis',(0.,0.,1.));
#3788=DIRECTION('ref_axis',(1.,0.,0.));
#3789=DIRECTION('center_axis',(0.,-1.,0.));
#3790=DIRECTION('ref_axis',(1.,0.,0.));
#3791=DIRECTION('',(-1.,0.,0.));
#3792=DIRECTION('',(0.,0.,1.));
#3793=DIRECTION('',(1.,0.,0.));
#3794=DIRECTION('',(0.,0.,1.));
#3795=DIRECTION('center_axis',(-1.,0.,0.));
#3796=DIRECTION('ref_axis',(0.,-1.,0.));
#3797=DIRECTION('',(0.,1.,0.));
#3798=DIRECTION('',(0.,-1.,0.));
#3799=DIRECTION('',(0.,0.,1.));
#3800=DIRECTION('center_axis',(0.,1.,0.));
#3801=DIRECTION('ref_axis',(-1.,0.,0.));
#3802=DIRECTION('',(1.,0.,0.));
#3803=DIRECTION('',(-1.,0.,0.));
#3804=DIRECTION('',(0.,0.,1.));
#3805=DIRECTION('center_axis',(1.,0.,0.));
#3806=DIRECTION('ref_axis',(0.,1.,0.));
#3807=DIRECTION('',(0.,-1.,0.));
#3808=DIRECTION('',(0.,1.,0.));
#3809=DIRECTION('center_axis',(0.,0.,1.));
#3810=DIRECTION('ref_axis',(1.,0.,0.));
#3811=DIRECTION('center_axis',(0.,0.,1.));
#3812=DIRECTION('ref_axis',(1.,0.,0.));
#3813=DIRECTION('center_axis',(0.,0.,1.));
#3814=DIRECTION('ref_axis',(1.,0.,0.));
#3815=DIRECTION('',(0.,0.,1.));
#3816=DIRECTION('center_axis',(0.,0.,-1.));
#3817=DIRECTION('ref_axis',(1.,0.,0.));
#3818=DIRECTION('center_axis',(0.,0.,1.));
#3819=DIRECTION('ref_axis',(1.,0.,0.));
#3820=DIRECTION('center_axis',(0.,0.,1.));
#3821=DIRECTION('ref_axis',(1.,0.,0.));
#3822=DIRECTION('',(0.,0.,1.));
#3823=DIRECTION('center_axis',(0.,0.,-1.));
#3824=DIRECTION('ref_axis',(1.,0.,0.));
#3825=DIRECTION('center_axis',(0.,0.,1.));
#3826=DIRECTION('ref_axis',(1.,0.,0.));
#3827=DIRECTION('center_axis',(0.,0.,1.));
#3828=DIRECTION('ref_axis',(1.,0.,0.));
#3829=DIRECTION('',(0.,0.,1.));
#3830=DIRECTION('center_axis',(0.,0.,-1.));
#3831=DIRECTION('ref_axis',(1.,0.,0.));
#3832=DIRECTION('center_axis',(0.,0.,1.));
#3833=DIRECTION('ref_axis',(1.,0.,0.));
#3834=DIRECTION('center_axis',(0.,0.,1.));
#3835=DIRECTION('ref_axis',(1.,0.,0.));
#3836=DIRECTION('',(0.,0.,1.));
#3837=DIRECTION('center_axis',(0.,0.,-1.));
#3838=DIRECTION('ref_axis',(1.,0.,0.));
#3839=DIRECTION('center_axis',(0.,0.,1.));
#3840=DIRECTION('ref_axis',(1.,0.,0.));
#3841=DIRECTION('center_axis',(0.,0.,1.));
#3842=DIRECTION('ref_axis',(1.,0.,0.));
#3843=DIRECTION('',(0.,0.,1.));
#3844=DIRECTION('center_axis',(0.,0.,-1.));
#3845=DIRECTION('ref_axis',(1.,0.,0.));
#3846=DIRECTION('center_axis',(0.,0.,1.));
#3847=DIRECTION('ref_axis',(1.,0.,0.));
#3848=DIRECTION('center_axis',(0.,0.,1.));
#3849=DIRECTION('ref_axis',(1.,0.,0.));
#3850=DIRECTION('',(0.,0.,1.));
#3851=DIRECTION('center_axis',(0.,0.,-1.));
#3852=DIRECTION('ref_axis',(1.,0.,0.));
#3853=DIRECTION('center_axis',(0.,0.,1.));
#3854=DIRECTION('ref_axis',(1.,0.,0.));
#3855=DIRECTION('center_axis',(0.,0.,1.));
#3856=DIRECTION('ref_axis',(1.,0.,0.));
#3857=DIRECTION('',(0.,0.,1.));
#3858=DIRECTION('center_axis',(0.,0.,-1.));
#3859=DIRECTION('ref_axis',(1.,0.,0.));
#3860=DIRECTION('center_axis',(0.,0.,1.));
#3861=DIRECTION('ref_axis',(1.,0.,0.));
#3862=DIRECTION('center_axis',(0.,0.,1.));
#3863=DIRECTION('ref_axis',(1.,0.,0.));
#3864=DIRECTION('',(0.,0.,1.));
#3865=DIRECTION('center_axis',(0.,0.,-1.));
#3866=DIRECTION('ref_axis',(1.,0.,0.));
#3867=DIRECTION('center_axis',(0.,0.,1.));
#3868=DIRECTION('ref_axis',(1.,0.,0.));
#3869=DIRECTION('center_axis',(0.,0.,1.));
#3870=DIRECTION('ref_axis',(1.,0.,0.));
#3871=DIRECTION('',(0.,0.,1.));
#3872=DIRECTION('center_axis',(0.,0.,-1.));
#3873=DIRECTION('ref_axis',(1.,0.,0.));
#3874=DIRECTION('center_axis',(0.,0.,1.));
#3875=DIRECTION('ref_axis',(1.,0.,0.));
#3876=DIRECTION('center_axis',(0.,0.,1.));
#3877=DIRECTION('ref_axis',(1.,0.,0.));
#3878=DIRECTION('',(0.,0.,1.));
#3879=DIRECTION('center_axis',(0.,0.,-1.));
#3880=DIRECTION('ref_axis',(1.,0.,0.));
#3881=DIRECTION('center_axis',(0.,0.,1.));
#3882=DIRECTION('ref_axis',(1.,0.,0.));
#3883=DIRECTION('center_axis',(0.,0.,1.));
#3884=DIRECTION('ref_axis',(1.,0.,0.));
#3885=DIRECTION('',(0.,0.,1.));
#3886=DIRECTION('center_axis',(0.,0.,-1.));
#3887=DIRECTION('ref_axis',(1.,0.,0.));
#3888=DIRECTION('center_axis',(0.,0.,1.));
#3889=DIRECTION('ref_axis',(1.,0.,0.));
#3890=DIRECTION('center_axis',(0.,0.,1.));
#3891=DIRECTION('ref_axis',(1.,0.,0.));
#3892=DIRECTION('',(0.,0.,1.));
#3893=DIRECTION('center_axis',(0.,0.,-1.));
#3894=DIRECTION('ref_axis',(1.,0.,0.));
#3895=DIRECTION('center_axis',(0.,0.,1.));
#3896=DIRECTION('ref_axis',(1.,0.,0.));
#3897=DIRECTION('center_axis',(0.,0.,1.));
#3898=DIRECTION('ref_axis',(1.,0.,0.));
#3899=DIRECTION('',(0.,0.,1.));
#3900=DIRECTION('center_axis',(0.,0.,-1.));
#3901=DIRECTION('ref_axis',(1.,0.,0.));
#3902=DIRECTION('center_axis',(0.,0.,1.));
#3903=DIRECTION('ref_axis',(1.,0.,0.));
#3904=DIRECTION('center_axis',(0.,0.,1.));
#3905=DIRECTION('ref_axis',(1.,0.,0.));
#3906=DIRECTION('',(0.,0.,1.));
#3907=DIRECTION('center_axis',(0.,0.,-1.));
#3908=DIRECTION('ref_axis',(1.,0.,0.));
#3909=DIRECTION('center_axis',(0.,0.,1.));
#3910=DIRECTION('ref_axis',(1.,0.,0.));
#3911=DIRECTION('center_axis',(0.,0.,1.));
#3912=DIRECTION('ref_axis',(1.,0.,0.));
#3913=DIRECTION('',(0.,0.,1.));
#3914=DIRECTION('center_axis',(0.,0.,-1.));
#3915=DIRECTION('ref_axis',(1.,0.,0.));
#3916=DIRECTION('center_axis',(0.,0.,1.));
#3917=DIRECTION('ref_axis',(1.,0.,0.));
#3918=DIRECTION('center_axis',(0.,0.,1.));
#3919=DIRECTION('ref_axis',(1.,0.,0.));
#3920=DIRECTION('',(0.,0.,1.));
#3921=DIRECTION('center_axis',(0.,0.,-1.));
#3922=DIRECTION('ref_axis',(1.,0.,0.));
#3923=DIRECTION('center_axis',(0.,0.,1.));
#3924=DIRECTION('ref_axis',(1.,0.,0.));
#3925=DIRECTION('center_axis',(0.,0.,1.));
#3926=DIRECTION('ref_axis',(1.,0.,0.));
#3927=DIRECTION('',(0.,0.,1.));
#3928=DIRECTION('center_axis',(0.,0.,-1.));
#3929=DIRECTION('ref_axis',(1.,0.,0.));
#3930=DIRECTION('center_axis',(0.,0.,1.));
#3931=DIRECTION('ref_axis',(1.,0.,0.));
#3932=DIRECTION('center_axis',(0.,0.,1.));
#3933=DIRECTION('ref_axis',(1.,0.,0.));
#3934=DIRECTION('',(0.,0.,1.));
#3935=DIRECTION('center_axis',(0.,0.,-1.));
#3936=DIRECTION('ref_axis',(1.,0.,0.));
#3937=DIRECTION('center_axis',(0.,0.,1.));
#3938=DIRECTION('ref_axis',(1.,0.,0.));
#3939=DIRECTION('center_axis',(0.,0.,1.));
#3940=DIRECTION('ref_axis',(1.,0.,0.));
#3941=DIRECTION('',(0.,0.,1.));
#3942=DIRECTION('center_axis',(0.,0.,-1.));
#3943=DIRECTION('ref_axis',(1.,0.,0.));
#3944=DIRECTION('center_axis',(0.,0.,1.));
#3945=DIRECTION('ref_axis',(1.,0.,0.));
#3946=DIRECTION('center_axis',(0.,0.,1.));
#3947=DIRECTION('ref_axis',(1.,0.,0.));
#3948=DIRECTION('',(0.,0.,1.));
#3949=DIRECTION('center_axis',(0.,0.,-1.));
#3950=DIRECTION('ref_axis',(1.,0.,0.));
#3951=DIRECTION('center_axis',(0.,0.,1.));
#3952=DIRECTION('ref_axis',(1.,0.,0.));
#3953=DIRECTION('center_axis',(0.,0.,1.));
#3954=DIRECTION('ref_axis',(1.,0.,0.));
#3955=DIRECTION('',(0.,0.,1.));
#3956=DIRECTION('center_axis',(0.,0.,-1.));
#3957=DIRECTION('ref_axis',(1.,0.,0.));
#3958=DIRECTION('center_axis',(0.,0.,1.));
#3959=DIRECTION('ref_axis',(1.,0.,0.));
#3960=DIRECTION('center_axis',(0.,0.,1.));
#3961=DIRECTION('ref_axis',(1.,0.,0.));
#3962=DIRECTION('',(0.,0.,1.));
#3963=DIRECTION('center_axis',(0.,0.,-1.));
#3964=DIRECTION('ref_axis',(1.,0.,0.));
#3965=DIRECTION('center_axis',(0.,0.,1.));
#3966=DIRECTION('ref_axis',(1.,0.,0.));
#3967=DIRECTION('center_axis',(0.,0.,1.));
#3968=DIRECTION('ref_axis',(1.,0.,0.));
#3969=DIRECTION('',(0.,0.,1.));
#3970=DIRECTION('center_axis',(0.,0.,-1.));
#3971=DIRECTION('ref_axis',(1.,0.,0.));
#3972=DIRECTION('center_axis',(0.,0.,1.));
#3973=DIRECTION('ref_axis',(1.,0.,0.));
#3974=DIRECTION('center_axis',(0.,0.,1.));
#3975=DIRECTION('ref_axis',(1.,0.,0.));
#3976=DIRECTION('',(0.,0.,1.));
#3977=DIRECTION('center_axis',(0.,0.,-1.));
#3978=DIRECTION('ref_axis',(1.,0.,0.));
#3979=DIRECTION('center_axis',(0.,0.,1.));
#3980=DIRECTION('ref_axis',(1.,0.,0.));
#3981=DIRECTION('center_axis',(0.,0.,1.));
#3982=DIRECTION('ref_axis',(1.,0.,0.));
#3983=DIRECTION('',(0.,0.,1.));
#3984=DIRECTION('center_axis',(0.,0.,-1.));
#3985=DIRECTION('ref_axis',(1.,0.,0.));
#3986=DIRECTION('center_axis',(0.,1.,0.));
#3987=DIRECTION('ref_axis',(-1.,0.,0.));
#3988=DIRECTION('',(-1.,0.,0.));
#3989=DIRECTION('',(0.,0.,1.));
#3990=DIRECTION('',(-1.,0.,0.));
#3991=DIRECTION('',(0.,0.,1.));
#3992=DIRECTION('center_axis',(1.,0.,0.));
#3993=DIRECTION('ref_axis',(0.,1.,0.));
#3994=DIRECTION('',(0.,1.,0.));
#3995=DIRECTION('',(0.,1.,0.));
#3996=DIRECTION('',(0.,0.,1.));
#3997=DIRECTION('center_axis',(0.,-1.,0.));
#3998=DIRECTION('ref_axis',(1.,0.,0.));
#3999=DIRECTION('',(1.,0.,0.));
#4000=DIRECTION('',(1.,0.,0.));
#4001=DIRECTION('',(0.,0.,1.));
#4002=DIRECTION('center_axis',(-1.,0.,0.));
#4003=DIRECTION('ref_axis',(0.,-1.,0.));
#4004=DIRECTION('',(0.,-1.,0.));
#4005=DIRECTION('',(0.,-1.,0.));
#4006=DIRECTION('center_axis',(0.,0.,1.));
#4007=DIRECTION('ref_axis',(1.,0.,0.));
#4008=DIRECTION('center_axis',(0.,0.,1.));
#4009=DIRECTION('ref_axis',(1.,0.,0.));
#4010=DIRECTION('axis',(0.,0.,1.));
#4011=DIRECTION('refdir',(1.,0.,0.));
#4012=DIRECTION('center_axis',(1.,0.,0.));
#4013=DIRECTION('ref_axis',(0.,0.,-1.));
#4014=DIRECTION('',(0.,-0.707106781186547,-0.707106781186548));
#4015=DIRECTION('',(0.,-1.,0.));
#4016=DIRECTION('',(0.,-0.707106781186547,0.707106781186548));
#4017=DIRECTION('',(0.,0.,1.));
#4018=DIRECTION('',(0.,0.707106781186547,0.707106781186548));
#4019=DIRECTION('',(0.,1.,0.));
#4020=DIRECTION('',(0.,0.707106781186547,-0.707106781186548));
#4021=DIRECTION('',(0.,0.,-1.));
#4022=DIRECTION('center_axis',(0.,0.707106781186548,-0.707106781186547));
#4023=DIRECTION('ref_axis',(-1.,0.,0.));
#4024=DIRECTION('',(1.,0.,0.));
#4025=DIRECTION('',(0.,-0.707106781186547,-0.707106781186548));
#4026=DIRECTION('',(-1.,0.,0.));
#4027=DIRECTION('center_axis',(0.,1.,0.));
#4028=DIRECTION('ref_axis',(-1.,0.,0.));
#4029=DIRECTION('',(-1.,0.,0.));
#4030=DIRECTION('',(0.,0.,-1.));
#4031=DIRECTION('center_axis',(0.,0.707106781186548,0.707106781186547));
#4032=DIRECTION('ref_axis',(1.,0.,0.));
#4033=DIRECTION('',(1.,0.,0.));
#4034=DIRECTION('',(0.,0.707106781186547,-0.707106781186548));
#4035=DIRECTION('center_axis',(0.,0.,1.));
#4036=DIRECTION('ref_axis',(1.,0.,0.));
#4037=DIRECTION('',(-1.,0.,0.));
#4038=DIRECTION('',(0.,1.,0.));
#4039=DIRECTION('center_axis',(1.,0.,0.));
#4040=DIRECTION('ref_axis',(0.,0.,-1.));
#4041=DIRECTION('',(0.,-0.707106781186547,0.707106781186548));
#4042=DIRECTION('',(0.,-1.,0.));
#4043=DIRECTION('',(0.,0.707106781186547,0.707106781186548));
#4044=DIRECTION('',(0.,0.,1.));
#4045=DIRECTION('center_axis',(0.,0.,1.));
#4046=DIRECTION('ref_axis',(1.,0.,0.));
#4047=DIRECTION('',(1.,0.,0.));
#4048=DIRECTION('center_axis',(0.,-0.707106781186548,0.707106781186547));
#4049=DIRECTION('ref_axis',(1.,0.,0.));
#4050=DIRECTION('',(1.,0.,0.));
#4051=DIRECTION('center_axis',(0.,-0.707106781186548,-0.707106781186547));
#4052=DIRECTION('ref_axis',(-1.,0.,0.));
#4053=DIRECTION('',(-1.,0.,0.));
#4054=DIRECTION('center_axis',(0.,-1.,0.));
#4055=DIRECTION('ref_axis',(1.,0.,0.));
#4056=DIRECTION('axis',(0.,0.,1.));
#4057=DIRECTION('refdir',(1.,0.,0.));
#4058=DIRECTION('center_axis',(0.,0.,1.));
#4059=DIRECTION('ref_axis',(1.,0.,0.));
#4060=DIRECTION('',(0.,0.,1.));
#4061=DIRECTION('center_axis',(0.,0.,1.));
#4062=DIRECTION('ref_axis',(1.,0.,0.));
#4063=DIRECTION('',(0.,0.,1.));
#4064=DIRECTION('center_axis',(0.,0.,-1.));
#4065=DIRECTION('ref_axis',(1.,0.,0.));
#4066=DIRECTION('center_axis',(0.,0.,1.));
#4067=DIRECTION('ref_axis',(1.,0.,0.));
#4068=DIRECTION('',(0.,0.,1.));
#4069=DIRECTION('center_axis',(0.,0.,1.));
#4070=DIRECTION('ref_axis',(1.,0.,0.));
#4071=DIRECTION('',(0.,0.,1.));
#4072=DIRECTION('center_axis',(0.,0.,-1.));
#4073=DIRECTION('ref_axis',(1.,0.,0.));
#4074=DIRECTION('center_axis',(0.,-0.707106781186547,-0.707106781186548));
#4075=DIRECTION('ref_axis',(0.,0.707106781186548,-0.707106781186547));
#4076=DIRECTION('center_axis',(0.,-1.,0.));
#4077=DIRECTION('ref_axis',(1.,0.,0.));
#4078=DIRECTION('',(1.,0.,0.));
#4079=DIRECTION('',(0.,0.,1.));
#4080=DIRECTION('',(1.,0.,0.));
#4081=DIRECTION('',(0.,0.,1.));
#4082=DIRECTION('center_axis',(1.,0.,0.));
#4083=DIRECTION('ref_axis',(0.,1.,0.));
#4084=DIRECTION('',(0.,1.,0.));
#4085=DIRECTION('',(0.,1.,0.));
#4086=DIRECTION('',(0.,0.,1.));
#4087=DIRECTION('center_axis',(0.,1.,0.));
#4088=DIRECTION('ref_axis',(-1.,0.,0.));
#4089=DIRECTION('',(-1.,0.,0.));
#4090=DIRECTION('',(-1.,0.,0.));
#4091=DIRECTION('',(0.,0.,1.));
#4092=DIRECTION('center_axis',(-1.,0.,0.));
#4093=DIRECTION('ref_axis',(0.,-1.,0.));
#4094=DIRECTION('',(0.,-1.,0.));
#4095=DIRECTION('',(0.,-1.,0.));
#4096=DIRECTION('center_axis',(0.,0.,1.));
#4097=DIRECTION('ref_axis',(1.,0.,0.));
#4098=DIRECTION('center_axis',(0.,0.,1.));
#4099=DIRECTION('ref_axis',(1.,0.,0.));
#4100=DIRECTION('center_axis',(0.,0.,-1.));
#4101=DIRECTION('ref_axis',(1.,0.,0.));
#4102=DIRECTION('',(0.,0.,1.));
#4103=DIRECTION('center_axis',(0.,0.,1.));
#4104=DIRECTION('ref_axis',(1.,0.,0.));
#4105=DIRECTION('center_axis',(0.,0.,1.));
#4106=DIRECTION('ref_axis',(1.,0.,0.));
#4107=DIRECTION('center_axis',(0.,0.,1.));
#4108=DIRECTION('ref_axis',(1.,0.,0.));
#4109=DIRECTION('center_axis',(0.,0.,1.));
#4110=DIRECTION('ref_axis',(1.,0.,0.));
#4111=DIRECTION('center_axis',(0.,0.707106781186547,-0.707106781186548));
#4112=DIRECTION('ref_axis',(0.,0.707106781186548,0.707106781186547));
#4113=DIRECTION('center_axis',(0.,0.,-1.));
#4114=DIRECTION('ref_axis',(1.,0.,0.));
#4115=DIRECTION('',(0.,0.,1.));
#4116=DIRECTION('center_axis',(0.,0.,1.));
#4117=DIRECTION('ref_axis',(1.,0.,0.));
#4118=DIRECTION('center_axis',(0.,0.,1.));
#4119=DIRECTION('ref_axis',(1.,0.,0.));
#4120=DIRECTION('center_axis',(0.,0.,1.));
#4121=DIRECTION('ref_axis',(1.,0.,0.));
#4122=DIRECTION('center_axis',(0.,-0.707106781186547,-0.707106781186548));
#4123=DIRECTION('ref_axis',(0.,0.707106781186548,-0.707106781186547));
#4124=DIRECTION('',(-1.,0.,0.));
#4125=DIRECTION('',(0.,-0.707106781186548,0.707106781186547));
#4126=DIRECTION('',(1.,0.,0.));
#4127=DIRECTION('',(0.,0.707106781186548,-0.707106781186547));
#4128=DIRECTION('',(-1.,0.,0.));
#4129=DIRECTION('center_axis',(0.,0.,1.));
#4130=DIRECTION('ref_axis',(1.,0.,0.));
#4131=DIRECTION('',(1.,0.,0.));
#4132=DIRECTION('',(0.,1.,0.));
#4133=DIRECTION('center_axis',(0.,0.707106781186547,-0.707106781186548));
#4134=DIRECTION('ref_axis',(0.,0.707106781186548,0.707106781186547));
#4135=DIRECTION('',(1.,0.,0.));
#4136=DIRECTION('',(0.,0.707106781186548,0.707106781186547));
#4137=DIRECTION('',(0.,-0.707106781186548,-0.707106781186547));
#4138=DIRECTION('',(1.,0.,0.));
#4139=DIRECTION('center_axis',(0.,0.,1.));
#4140=DIRECTION('ref_axis',(1.,0.,0.));
#4141=DIRECTION('',(-1.,0.,0.));
#4142=DIRECTION('',(0.,-1.,0.));
#4143=DIRECTION('center_axis',(0.,0.,1.));
#4144=DIRECTION('ref_axis',(1.,0.,0.));
#4145=DIRECTION('center_axis',(0.,0.,1.));
#4146=DIRECTION('ref_axis',(1.,0.,0.));
#4147=DIRECTION('',(0.,0.,1.));
#4148=DIRECTION('center_axis',(0.,0.,1.));
#4149=DIRECTION('ref_axis',(1.,0.,0.));
#4150=DIRECTION('center_axis',(0.,0.,1.));
#4151=DIRECTION('ref_axis',(1.,0.,0.));
#4152=DIRECTION('',(0.,0.,1.));
#4153=DIRECTION('center_axis',(0.,0.,1.));
#4154=DIRECTION('ref_axis',(1.,0.,0.));
#4155=DIRECTION('',(0.,-1.,0.));
#4156=DIRECTION('',(1.,0.,0.));
#4157=DIRECTION('center_axis',(0.,0.,1.));
#4158=DIRECTION('ref_axis',(1.,0.,0.));
#4159=DIRECTION('',(0.,1.,0.));
#4160=DIRECTION('',(-1.,0.,0.));
#4161=DIRECTION('center_axis',(-1.,0.,0.));
#4162=DIRECTION('ref_axis',(0.,-1.,0.));
#4163=DIRECTION('',(0.,0.,1.));
#4164=DIRECTION('',(0.,-1.,0.));
#4165=DIRECTION('',(0.,0.,1.));
#4166=DIRECTION('center_axis',(0.,1.,0.));
#4167=DIRECTION('ref_axis',(-1.,0.,0.));
#4168=DIRECTION('',(-1.,0.,0.));
#4169=DIRECTION('',(0.,0.,1.));
#4170=DIRECTION('center_axis',(1.,0.,0.));
#4171=DIRECTION('ref_axis',(0.,1.,0.));
#4172=DIRECTION('',(0.,0.,1.));
#4173=DIRECTION('',(0.,1.,0.));
#4174=DIRECTION('center_axis',(0.,-1.,0.));
#4175=DIRECTION('ref_axis',(1.,0.,0.));
#4176=DIRECTION('',(1.,0.,0.));
#4177=DIRECTION('center_axis',(0.,0.,1.));
#4178=DIRECTION('ref_axis',(1.,0.,0.));
#4179=DIRECTION('center_axis',(0.,0.,1.));
#4180=DIRECTION('ref_axis',(-1.,0.,0.));
#4181=DIRECTION('',(-1.,0.,0.));
#4182=DIRECTION('',(0.,-1.,0.));
#4183=DIRECTION('',(-1.,0.,0.));
#4184=DIRECTION('',(0.,-1.,0.));
#4185=DIRECTION('center_axis',(1.,0.,0.));
#4186=DIRECTION('ref_axis',(0.,0.,1.));
#4187=DIRECTION('',(0.,0.,1.));
#4188=DIRECTION('',(0.,0.,1.));
#4189=DIRECTION('',(0.,-1.,0.));
#4190=DIRECTION('center_axis',(0.,0.,-1.));
#4191=DIRECTION('ref_axis',(1.,0.,0.));
#4192=DIRECTION('',(1.,0.,0.));
#4193=DIRECTION('',(1.,0.,0.));
#4194=DIRECTION('',(0.,-1.,0.));
#4195=DIRECTION('center_axis',(-1.,0.,0.));
#4196=DIRECTION('ref_axis',(0.,0.,-1.));
#4197=DIRECTION('',(0.,0.,-1.));
#4198=DIRECTION('',(0.,0.,-1.));
#4199=DIRECTION('center_axis',(0.,-1.,0.));
#4200=DIRECTION('ref_axis',(0.,0.,-1.));
#4201=DIRECTION('center_axis',(0.,-1.,0.));
#4202=DIRECTION('ref_axis',(1.,0.,0.));
#4203=DIRECTION('center_axis',(0.,0.,1.));
#4204=DIRECTION('ref_axis',(1.,0.,0.));
#4205=DIRECTION('',(1.,0.,0.));
#4206=DIRECTION('',(0.,1.,0.));
#4207=DIRECTION('',(1.,0.,0.));
#4208=DIRECTION('',(0.,1.,0.));
#4209=DIRECTION('center_axis',(-1.,0.,0.));
#4210=DIRECTION('ref_axis',(0.,0.,1.));
#4211=DIRECTION('',(0.,0.,1.));
#4212=DIRECTION('',(0.,0.,1.));
#4213=DIRECTION('',(0.,1.,0.));
#4214=DIRECTION('center_axis',(0.,0.,-1.));
#4215=DIRECTION('ref_axis',(-1.,0.,0.));
#4216=DIRECTION('',(-1.,0.,0.));
#4217=DIRECTION('',(-1.,0.,0.));
#4218=DIRECTION('',(0.,1.,0.));
#4219=DIRECTION('center_axis',(1.,0.,0.));
#4220=DIRECTION('ref_axis',(0.,0.,-1.));
#4221=DIRECTION('',(0.,0.,-1.));
#4222=DIRECTION('',(0.,0.,-1.));
#4223=DIRECTION('center_axis',(0.,1.,0.));
#4224=DIRECTION('ref_axis',(0.,0.,1.));
#4225=DIRECTION('center_axis',(0.,1.,0.));
#4226=DIRECTION('ref_axis',(-1.,0.,0.));
#4227=DIRECTION('axis',(0.,0.,1.));
#4228=DIRECTION('refdir',(1.,0.,0.));
#4229=DIRECTION('center_axis',(0.,1.,0.));
#4230=DIRECTION('ref_axis',(0.,0.,1.));
#4231=DIRECTION('center_axis',(0.,-1.,0.));
#4232=DIRECTION('ref_axis',(1.,0.,0.));
#4233=DIRECTION('center_axis',(0.,-1.,0.));
#4234=DIRECTION('ref_axis',(1.,0.,0.));
#4235=DIRECTION('center_axis',(0.,-1.,0.));
#4236=DIRECTION('ref_axis',(1.,0.,0.));
#4237=DIRECTION('',(0.707106781186548,0.707106781186547,8.65956056235494E-17));
#4238=DIRECTION('center_axis',(0.,-1.,0.));
#4239=DIRECTION('ref_axis',(1.,0.,0.));
#4240=DIRECTION('center_axis',(0.,-1.,0.));
#4241=DIRECTION('ref_axis',(1.,0.,0.));
#4242=DIRECTION('',(0.,1.,0.));
#4243=DIRECTION('center_axis',(0.,1.,0.));
#4244=DIRECTION('ref_axis',(1.,0.,0.));
#4245=DIRECTION('center_axis',(0.,-1.,0.));
#4246=DIRECTION('ref_axis',(1.,0.,0.));
#4247=DIRECTION('',(-0.707106781186547,0.707106781186548,-8.65956056235493E-17));
#4248=DIRECTION('center_axis',(0.,-1.,0.));
#4249=DIRECTION('ref_axis',(0.,0.,-1.));
#4250=DIRECTION('center_axis',(0.,-1.,0.));
#4251=DIRECTION('ref_axis',(1.,0.,0.));
#4252=DIRECTION('center_axis',(0.,1.,0.));
#4253=DIRECTION('ref_axis',(1.,0.,0.));
#4254=DIRECTION('center_axis',(0.,1.,0.));
#4255=DIRECTION('ref_axis',(1.,0.,0.));
#4256=DIRECTION('',(-0.447213595499958,0.894427190999916,-5.47678698264203E-17));
#4257=DIRECTION('center_axis',(0.,-1.,0.));
#4258=DIRECTION('ref_axis',(1.,0.,0.));
#4259=DIRECTION('center_axis',(0.,1.,0.));
#4260=DIRECTION('ref_axis',(1.,0.,0.));
#4261=DIRECTION('',(0.,1.,0.));
#4262=DIRECTION('center_axis',(0.,1.,0.));
#4263=DIRECTION('ref_axis',(1.,0.,0.));
#4264=DIRECTION('center_axis',(0.,-1.,0.));
#4265=DIRECTION('ref_axis',(1.,0.,0.));
#4266=DIRECTION('',(-0.707106781186547,0.707106781186548,-8.65956056235493E-17));
#4267=DIRECTION('center_axis',(0.,-1.,0.));
#4268=DIRECTION('ref_axis',(0.,0.,-1.));
#4269=DIRECTION('center_axis',(0.866025403784439,0.,-0.5));
#4270=DIRECTION('ref_axis',(0.5,0.,0.866025403784439));
#4271=DIRECTION('',(-0.5,0.,-0.866025403784439));
#4272=DIRECTION('',(0.,-1.,0.));
#4273=DIRECTION('',(0.5,0.,0.866025403784439));
#4274=DIRECTION('',(0.,-1.,0.));
#4275=DIRECTION('center_axis',(1.92296268638356E-16,0.,-1.));
#4276=DIRECTION('ref_axis',(1.,0.,1.92296268638356E-16));
#4277=DIRECTION('',(-1.,0.,-1.92296268638356E-16));
#4278=DIRECTION('',(0.,-1.,0.));
#4279=DIRECTION('',(1.,0.,1.92296268638356E-16));
#4280=DIRECTION('center_axis',(-0.866025403784439,0.,-0.5));
#4281=DIRECTION('ref_axis',(0.5,0.,-0.866025403784439));
#4282=DIRECTION('',(-0.5,0.,0.866025403784438));
#4283=DIRECTION('',(0.,-1.,0.));
#4284=DIRECTION('',(0.5,0.,-0.866025403784438));
#4285=DIRECTION('center_axis',(-0.866025403784439,0.,0.5));
#4286=DIRECTION('ref_axis',(-0.5,0.,-0.866025403784439));
#4287=DIRECTION('',(0.5,0.,0.866025403784439));
#4288=DIRECTION('',(0.,-1.,0.));
#4289=DIRECTION('',(-0.5,0.,-0.866025403784439));
#4290=DIRECTION('center_axis',(-1.92296268638356E-16,0.,1.));
#4291=DIRECTION('ref_axis',(-1.,0.,-1.92296268638356E-16));
#4292=DIRECTION('',(1.,0.,1.92296268638356E-16));
#4293=DIRECTION('',(0.,-1.,0.));
#4294=DIRECTION('',(-1.,0.,-1.92296268638356E-16));
#4295=DIRECTION('center_axis',(0.866025403784439,0.,0.5));
#4296=DIRECTION('ref_axis',(-0.5,0.,0.866025403784439));
#4297=DIRECTION('',(0.5,0.,-0.866025403784439));
#4298=DIRECTION('',(-0.5,0.,0.866025403784439));
#4299=DIRECTION('center_axis',(0.,1.,0.));
#4300=DIRECTION('ref_axis',(1.,0.,0.));
#4301=DIRECTION('center_axis',(0.,-1.,0.));
#4302=DIRECTION('ref_axis',(0.,0.,-1.));
#4303=DIRECTION('axis',(0.,0.,1.));
#4304=DIRECTION('refdir',(1.,0.,0.));
#4305=DIRECTION('center_axis',(0.,0.,1.));
#4306=DIRECTION('ref_axis',(1.,0.,0.));
#4307=DIRECTION('center_axis',(0.,0.,1.));
#4308=DIRECTION('ref_axis',(1.,0.,0.));
#4309=DIRECTION('',(0.,0.,1.));
#4310=DIRECTION('center_axis',(0.,0.,-1.));
#4311=DIRECTION('ref_axis',(1.,0.,0.));
#4312=DIRECTION('center_axis',(0.,0.,1.));
#4313=DIRECTION('ref_axis',(1.,0.,0.));
#4314=DIRECTION('center_axis',(0.,0.,1.));
#4315=DIRECTION('ref_axis',(1.,0.,0.));
#4316=DIRECTION('',(0.,0.,1.));
#4317=DIRECTION('center_axis',(0.,0.,-1.));
#4318=DIRECTION('ref_axis',(1.,0.,0.));
#4319=DIRECTION('center_axis',(0.,0.,1.));
#4320=DIRECTION('ref_axis',(1.,0.,0.));
#4321=DIRECTION('center_axis',(0.,0.,1.));
#4322=DIRECTION('ref_axis',(1.,0.,0.));
#4323=DIRECTION('',(0.,0.,1.));
#4324=DIRECTION('center_axis',(0.,0.,-1.));
#4325=DIRECTION('ref_axis',(1.,0.,0.));
#4326=DIRECTION('center_axis',(0.,0.,1.));
#4327=DIRECTION('ref_axis',(1.,0.,0.));
#4328=DIRECTION('center_axis',(0.,0.,1.));
#4329=DIRECTION('ref_axis',(1.,0.,0.));
#4330=DIRECTION('',(0.,0.,1.));
#4331=DIRECTION('center_axis',(0.,0.,-1.));
#4332=DIRECTION('ref_axis',(1.,0.,0.));
#4333=DIRECTION('center_axis',(0.,1.,0.));
#4334=DIRECTION('ref_axis',(-1.,0.,0.));
#4335=DIRECTION('',(-1.,0.,0.));
#4336=DIRECTION('',(0.,0.,1.));
#4337=DIRECTION('',(-1.,0.,0.));
#4338=DIRECTION('',(0.,0.,1.));
#4339=DIRECTION('center_axis',(1.,0.,0.));
#4340=DIRECTION('ref_axis',(0.,1.,0.));
#4341=DIRECTION('',(0.,1.,0.));
#4342=DIRECTION('',(0.,1.,0.));
#4343=DIRECTION('',(0.,0.,1.));
#4344=DIRECTION('center_axis',(0.,-1.,0.));
#4345=DIRECTION('ref_axis',(1.,0.,0.));
#4346=DIRECTION('',(1.,0.,0.));
#4347=DIRECTION('',(1.,0.,0.));
#4348=DIRECTION('',(0.,0.,1.));
#4349=DIRECTION('center_axis',(-1.,0.,0.));
#4350=DIRECTION('ref_axis',(0.,-1.,0.));
#4351=DIRECTION('',(0.,-1.,0.));
#4352=DIRECTION('',(0.,-1.,0.));
#4353=DIRECTION('center_axis',(0.,0.,1.));
#4354=DIRECTION('ref_axis',(1.,0.,0.));
#4355=DIRECTION('center_axis',(0.,0.,1.));
#4356=DIRECTION('ref_axis',(1.,0.,0.));
#4357=DIRECTION('axis',(0.,0.,1.));
#4358=DIRECTION('refdir',(1.,0.,0.));
#4359=DIRECTION('center_axis',(0.,0.,1.));
#4360=DIRECTION('ref_axis',(1.,0.,0.));
#4361=DIRECTION('center_axis',(0.,0.,1.));
#4362=DIRECTION('ref_axis',(1.,0.,0.));
#4363=DIRECTION('',(0.,0.,1.));
#4364=DIRECTION('center_axis',(0.,0.,-1.));
#4365=DIRECTION('ref_axis',(1.,0.,0.));
#4366=DIRECTION('center_axis',(0.,0.,1.));
#4367=DIRECTION('ref_axis',(1.,0.,0.));
#4368=DIRECTION('center_axis',(0.,0.,1.));
#4369=DIRECTION('ref_axis',(1.,0.,0.));
#4370=DIRECTION('center_axis',(0.,0.,1.));
#4371=DIRECTION('ref_axis',(1.,0.,0.));
#4372=DIRECTION('',(0.,0.,1.));
#4373=DIRECTION('center_axis',(0.,0.,-1.));
#4374=DIRECTION('ref_axis',(1.,0.,0.));
#4375=DIRECTION('center_axis',(0.,0.,1.));
#4376=DIRECTION('ref_axis',(1.,0.,0.));
#4377=DIRECTION('center_axis',(1.,0.,0.));
#4378=DIRECTION('ref_axis',(0.,1.22464679914735E-16,1.));
#4379=DIRECTION('',(-1.,0.,0.));
#4380=DIRECTION('center_axis',(-1.,0.,0.));
#4381=DIRECTION('ref_axis',(0.,0.,-1.));
#4382=DIRECTION('',(1.,0.,0.));
#4383=DIRECTION('center_axis',(1.,0.,0.));
#4384=DIRECTION('ref_axis',(0.,0.,-1.));
#4385=DIRECTION('center_axis',(1.,0.,0.));
#4386=DIRECTION('ref_axis',(0.,1.,0.));
#4387=DIRECTION('',(0.,0.,1.));
#4388=DIRECTION('',(0.,1.,0.));
#4389=DIRECTION('',(0.,0.,1.));
#4390=DIRECTION('center_axis',(0.,1.,0.));
#4391=DIRECTION('ref_axis',(-1.,0.,0.));
#4392=DIRECTION('',(0.,0.,1.));
#4393=DIRECTION('',(-1.,0.,0.));
#4394=DIRECTION('center_axis',(0.,-1.,0.));
#4395=DIRECTION('ref_axis',(1.,0.,0.));
#4396=DIRECTION('',(1.,0.,0.));
#4397=DIRECTION('',(0.,0.,1.));
#4398=DIRECTION('center_axis',(-1.,0.,0.));
#4399=DIRECTION('ref_axis',(0.,-1.,0.));
#4400=DIRECTION('',(0.,-1.,0.));
#4401=DIRECTION('center_axis',(0.,0.,1.));
#4402=DIRECTION('ref_axis',(1.,0.,0.));
#4403=DIRECTION('axis',(0.,0.,1.));
#4404=DIRECTION('refdir',(1.,0.,0.));
#4405=DIRECTION('center_axis',(1.,0.,0.));
#4406=DIRECTION('ref_axis',(0.,0.,-1.));
#4407=DIRECTION('center_axis',(1.,0.,0.));
#4408=DIRECTION('ref_axis',(0.,0.,-1.));
#4409=DIRECTION('',(-1.,0.,0.));
#4410=DIRECTION('center_axis',(1.,0.,0.));
#4411=DIRECTION('ref_axis',(0.,0.,-1.));
#4412=DIRECTION('center_axis',(1.,0.,0.));
#4413=DIRECTION('ref_axis',(0.,0.,-1.));
#4414=DIRECTION('center_axis',(1.,0.,0.));
#4415=DIRECTION('ref_axis',(0.,0.,-1.));
#4416=DIRECTION('axis',(0.,0.,1.));
#4417=DIRECTION('refdir',(1.,0.,0.));
#4418=DIRECTION('center_axis',(0.866025403784439,0.,-0.5));
#4419=DIRECTION('ref_axis',(0.5,0.,0.866025403784439));
#4420=DIRECTION('',(-0.5,0.,-0.866025403784439));
#4421=DIRECTION('',(0.,-1.,0.));
#4422=DIRECTION('',(0.5,0.,0.866025403784439));
#4423=DIRECTION('',(0.,-1.,0.));
#4424=DIRECTION('center_axis',(1.60246890531964E-16,0.,-1.));
#4425=DIRECTION('ref_axis',(1.,0.,1.60246890531964E-16));
#4426=DIRECTION('',(-1.,0.,-1.60246890531964E-16));
#4427=DIRECTION('',(0.,-1.,0.));
#4428=DIRECTION('',(1.,0.,1.60246890531964E-16));
#4429=DIRECTION('center_axis',(-0.866025403784439,0.,-0.5));
#4430=DIRECTION('ref_axis',(0.5,0.,-0.866025403784439));
#4431=DIRECTION('',(-0.5,0.,0.866025403784439));
#4432=DIRECTION('',(0.,-1.,0.));
#4433=DIRECTION('',(0.5,0.,-0.866025403784439));
#4434=DIRECTION('center_axis',(-0.866025403784439,0.,0.5));
#4435=DIRECTION('ref_axis',(-0.5,0.,-0.866025403784439));
#4436=DIRECTION('',(0.5,0.,0.866025403784439));
#4437=DIRECTION('',(0.,-1.,0.));
#4438=DIRECTION('',(-0.5,0.,-0.866025403784439));
#4439=DIRECTION('center_axis',(-1.60246890531964E-16,0.,1.));
#4440=DIRECTION('ref_axis',(-1.,0.,-1.60246890531964E-16));
#4441=DIRECTION('',(1.,0.,1.60246890531964E-16));
#4442=DIRECTION('',(0.,-1.,0.));
#4443=DIRECTION('',(-1.,0.,-1.60246890531964E-16));
#4444=DIRECTION('center_axis',(0.866025403784439,0.,0.5));
#4445=DIRECTION('ref_axis',(-0.5,0.,0.866025403784439));
#4446=DIRECTION('',(0.5,0.,-0.866025403784439));
#4447=DIRECTION('',(-0.5,0.,0.866025403784439));
#4448=DIRECTION('center_axis',(0.,1.,0.));
#4449=DIRECTION('ref_axis',(1.,0.,0.));
#4450=DIRECTION('center_axis',(0.,-1.,0.));
#4451=DIRECTION('ref_axis',(0.,0.,-1.));
#4452=DIRECTION('center_axis',(0.,1.,0.));
#4453=DIRECTION('ref_axis',(1.,0.,0.));
#4454=DIRECTION('center_axis',(0.,1.,0.));
#4455=DIRECTION('ref_axis',(1.,0.,0.));
#4456=DIRECTION('center_axis',(0.,1.,0.));
#4457=DIRECTION('ref_axis',(0.,0.,1.));
#4458=DIRECTION('center_axis',(0.,-1.,0.));
#4459=DIRECTION('ref_axis',(1.,0.,0.));
#4460=DIRECTION('center_axis',(0.,-1.,0.));
#4461=DIRECTION('ref_axis',(1.,0.,0.));
#4462=DIRECTION('center_axis',(0.,-1.,0.));
#4463=DIRECTION('ref_axis',(1.,0.,0.));
#4464=DIRECTION('',(0.707106781186547,0.707106781186548,8.65956056235493E-17));
#4465=DIRECTION('center_axis',(0.,-1.,0.));
#4466=DIRECTION('ref_axis',(1.,0.,0.));
#4467=DIRECTION('center_axis',(0.,-1.,0.));
#4468=DIRECTION('ref_axis',(1.,0.,0.));
#4469=DIRECTION('',(0.,1.,0.));
#4470=DIRECTION('center_axis',(0.,1.,0.));
#4471=DIRECTION('ref_axis',(1.,0.,0.));
#4472=DIRECTION('center_axis',(0.,-1.,0.));
#4473=DIRECTION('ref_axis',(1.,0.,0.));
#4474=DIRECTION('',(-0.707106781186547,0.707106781186548,-8.65956056235493E-17));
#4475=DIRECTION('center_axis',(0.,-1.,0.));
#4476=DIRECTION('ref_axis',(0.,0.,-1.));
#4477=DIRECTION('center_axis',(0.,-1.,0.));
#4478=DIRECTION('ref_axis',(1.,0.,0.));
#4479=DIRECTION('center_axis',(0.,1.,0.));
#4480=DIRECTION('ref_axis',(1.,0.,0.));
#4481=DIRECTION('center_axis',(0.,1.,0.));
#4482=DIRECTION('ref_axis',(1.,0.,0.));
#4483=DIRECTION('',(-0.447213595499958,0.894427190999916,-5.47678698264203E-17));
#4484=DIRECTION('center_axis',(0.,-1.,0.));
#4485=DIRECTION('ref_axis',(1.,0.,0.));
#4486=DIRECTION('',(0.,1.,0.));
#4487=DIRECTION('axis',(0.,0.,1.));
#4488=DIRECTION('refdir',(1.,0.,0.));
#4489=DIRECTION('center_axis',(0.,0.,1.));
#4490=DIRECTION('ref_axis',(1.,0.,0.));
#4491=DIRECTION('center_axis',(0.,0.,-1.));
#4492=DIRECTION('ref_axis',(1.,0.,0.));
#4493=DIRECTION('',(0.,0.,-1.));
#4494=DIRECTION('center_axis',(0.,0.,-1.));
#4495=DIRECTION('ref_axis',(1.,0.,0.));
#4496=DIRECTION('center_axis',(0.,0.,1.));
#4497=DIRECTION('ref_axis',(1.,0.,0.));
#4498=DIRECTION('center_axis',(0.,0.,1.));
#4499=DIRECTION('ref_axis',(1.,0.,0.));
#4500=DIRECTION('axis',(0.,0.,1.));
#4501=DIRECTION('refdir',(1.,0.,0.));
#4502=DIRECTION('center_axis',(0.,1.,0.));
#4503=DIRECTION('ref_axis',(1.,0.,0.));
#4504=DIRECTION('center_axis',(0.,-1.,0.));
#4505=DIRECTION('ref_axis',(1.,0.,0.));
#4506=DIRECTION('',(0.,-1.,0.));
#4507=DIRECTION('center_axis',(0.,-1.,0.));
#4508=DIRECTION('ref_axis',(1.,0.,0.));
#4509=DIRECTION('center_axis',(0.,1.,0.));
#4510=DIRECTION('ref_axis',(1.,0.,0.));
#4511=DIRECTION('center_axis',(0.,1.,0.));
#4512=DIRECTION('ref_axis',(1.,0.,0.));
#4513=DIRECTION('',(0.,-1.,0.));
#4514=DIRECTION('center_axis',(0.,1.,0.));
#4515=DIRECTION('ref_axis',(1.,0.,0.));
#4516=DIRECTION('center_axis',(0.,1.,0.));
#4517=DIRECTION('ref_axis',(1.,0.,0.));
#4518=DIRECTION('center_axis',(0.,1.,0.));
#4519=DIRECTION('ref_axis',(1.,0.,0.));
#4520=DIRECTION('axis',(0.,0.,1.));
#4521=DIRECTION('refdir',(1.,0.,0.));
#4522=DIRECTION('center_axis',(0.,1.,0.));
#4523=DIRECTION('ref_axis',(1.,0.,0.));
#4524=DIRECTION('',(0.866025403784439,-0.5,1.06057523872491E-16));
#4525=DIRECTION('center_axis',(0.,-1.,0.));
#4526=DIRECTION('ref_axis',(1.,0.,0.));
#4527=DIRECTION('center_axis',(0.,-1.,0.));
#4528=DIRECTION('ref_axis',(1.,0.,0.));
#4529=DIRECTION('center_axis',(0.,1.,0.));
#4530=DIRECTION('ref_axis',(1.,0.,0.));
#4531=DIRECTION('',(-0.866025403784439,-0.5,-1.06057523872491E-16));
#4532=DIRECTION('center_axis',(1.4792020664489E-16,0.,-1.));
#4533=DIRECTION('ref_axis',(-1.,0.,-1.4792020664489E-16));
#4534=DIRECTION('',(0.,1.,0.));
#4535=DIRECTION('',(0.,1.,0.));
#4536=DIRECTION('center_axis',(-0.866025403784439,0.,-0.5));
#4537=DIRECTION('ref_axis',(-0.5,0.,0.866025403784439));
#4538=DIRECTION('',(0.,1.,0.));
#4539=DIRECTION('center_axis',(-0.866025403784439,0.,0.5));
#4540=DIRECTION('ref_axis',(0.5,0.,0.866025403784439));
#4541=DIRECTION('',(0.,1.,0.));
#4542=DIRECTION('center_axis',(0.,1.,0.));
#4543=DIRECTION('ref_axis',(1.,0.,0.));
#4544=DIRECTION('center_axis',(0.,1.,0.));
#4545=DIRECTION('ref_axis',(1.,0.,0.));
#4546=DIRECTION('',(0.,-1.,0.));
#4547=DIRECTION('center_axis',(0.,1.,0.));
#4548=DIRECTION('ref_axis',(1.,0.,0.));
#4549=DIRECTION('center_axis',(-2.95840413289779E-16,0.,1.));
#4550=DIRECTION('ref_axis',(1.,0.,2.95840413289779E-16));
#4551=DIRECTION('',(0.,1.,0.));
#4552=DIRECTION('center_axis',(0.866025403784439,0.,-0.5));
#4553=DIRECTION('ref_axis',(-0.5,0.,-0.866025403784439));
#4554=DIRECTION('',(0.,1.,0.));
#4555=DIRECTION('center_axis',(0.866025403784439,0.,0.5));
#4556=DIRECTION('ref_axis',(0.5,0.,-0.866025403784439));
#4557=DIRECTION('center_axis',(0.,1.,0.));
#4558=DIRECTION('ref_axis',(1.,0.,0.));
#4559=DIRECTION('center_axis',(0.,1.,0.));
#4560=DIRECTION('ref_axis',(1.,0.,0.));
#4561=DIRECTION('axis',(0.,0.,1.));
#4562=DIRECTION('refdir',(1.,0.,0.));
#4563=DIRECTION('center_axis',(0.,0.,1.));
#4564=DIRECTION('ref_axis',(1.,0.,0.));
#4565=DIRECTION('',(0.,0.,-1.));
#4566=DIRECTION('center_axis',(0.,0.,-1.));
#4567=DIRECTION('ref_axis',(1.,0.,0.));
#4568=DIRECTION('',(0.,0.,1.));
#4569=DIRECTION('center_axis',(0.,0.,1.));
#4570=DIRECTION('ref_axis',(1.,0.,0.));
#4571=DIRECTION('center_axis',(0.,0.,1.));
#4572=DIRECTION('ref_axis',(-1.,-1.22464679914735E-16,0.));
#4573=DIRECTION('',(0.,0.,1.));
#4574=DIRECTION('center_axis',(0.,0.,1.));
#4575=DIRECTION('ref_axis',(1.,0.,0.));
#4576=DIRECTION('',(0.,0.,-1.));
#4577=DIRECTION('center_axis',(0.,0.,-1.));
#4578=DIRECTION('ref_axis',(1.,0.,0.));
#4579=DIRECTION('center_axis',(0.,0.,1.));
#4580=DIRECTION('ref_axis',(1.,0.,0.));
#4581=DIRECTION('',(0.,0.,-1.));
#4582=DIRECTION('center_axis',(0.,0.,-1.));
#4583=DIRECTION('ref_axis',(1.,0.,0.));
#4584=DIRECTION('',(0.,0.,1.));
#4585=DIRECTION('center_axis',(0.,0.,1.));
#4586=DIRECTION('ref_axis',(1.,0.,0.));
#4587=DIRECTION('center_axis',(0.,0.,1.));
#4588=DIRECTION('ref_axis',(1.,0.,0.));
#4589=DIRECTION('',(0.,0.,-1.));
#4590=DIRECTION('center_axis',(0.,0.,-1.));
#4591=DIRECTION('ref_axis',(1.,0.,0.));
#4592=DIRECTION('',(0.,0.,1.));
#4593=DIRECTION('center_axis',(0.,0.,1.));
#4594=DIRECTION('ref_axis',(1.,0.,0.));
#4595=DIRECTION('center_axis',(0.,0.,1.));
#4596=DIRECTION('ref_axis',(1.,0.,0.));
#4597=DIRECTION('',(0.,0.,-1.));
#4598=DIRECTION('center_axis',(0.,0.,-1.));
#4599=DIRECTION('ref_axis',(1.,0.,0.));
#4600=DIRECTION('',(0.,0.,1.));
#4601=DIRECTION('center_axis',(0.,0.,1.));
#4602=DIRECTION('ref_axis',(1.,0.,0.));
#4603=DIRECTION('center_axis',(0.,0.,1.));
#4604=DIRECTION('ref_axis',(1.,0.,0.));
#4605=DIRECTION('',(0.,0.,-1.));
#4606=DIRECTION('center_axis',(0.,0.,-1.));
#4607=DIRECTION('ref_axis',(1.,0.,0.));
#4608=DIRECTION('',(0.,0.,1.));
#4609=DIRECTION('center_axis',(0.,0.,1.));
#4610=DIRECTION('ref_axis',(1.,0.,0.));
#4611=DIRECTION('center_axis',(0.,0.,1.));
#4612=DIRECTION('ref_axis',(1.,0.,0.));
#4613=DIRECTION('center_axis',(0.,0.,1.));
#4614=DIRECTION('ref_axis',(1.,0.,0.));
#4615=DIRECTION('center_axis',(0.,0.,1.));
#4616=DIRECTION('ref_axis',(1.,0.,0.));
#4617=DIRECTION('center_axis',(0.,0.,1.));
#4618=DIRECTION('ref_axis',(1.,0.,0.));
#4619=DIRECTION('center_axis',(0.,0.,1.));
#4620=DIRECTION('ref_axis',(1.,0.,0.));
#4621=DIRECTION('center_axis',(0.,0.,1.));
#4622=DIRECTION('ref_axis',(1.,0.,0.));
#4623=DIRECTION('center_axis',(0.,0.,1.));
#4624=DIRECTION('ref_axis',(1.,0.,0.));
#4625=DIRECTION('center_axis',(0.,0.,-1.));
#4626=DIRECTION('ref_axis',(1.,0.,0.));
#4627=DIRECTION('center_axis',(0.,0.,1.));
#4628=DIRECTION('ref_axis',(1.,0.,0.));
#4629=DIRECTION('center_axis',(0.,0.,1.));
#4630=DIRECTION('ref_axis',(1.,0.,0.));
#4631=DIRECTION('center_axis',(0.,0.,1.));
#4632=DIRECTION('ref_axis',(1.,0.,0.));
#4633=DIRECTION('center_axis',(0.,0.,1.));
#4634=DIRECTION('ref_axis',(1.,0.,0.));
#4635=DIRECTION('center_axis',(0.,0.,1.));
#4636=DIRECTION('ref_axis',(1.,0.,0.));
#4637=DIRECTION('center_axis',(0.,0.,1.));
#4638=DIRECTION('ref_axis',(1.,0.,0.));
#4639=DIRECTION('center_axis',(0.,0.,1.));
#4640=DIRECTION('ref_axis',(1.,0.,0.));
#4641=DIRECTION('center_axis',(0.,0.,1.));
#4642=DIRECTION('ref_axis',(1.,0.,0.));
#4643=DIRECTION('center_axis',(0.,0.,1.));
#4644=DIRECTION('ref_axis',(1.,0.,0.));
#4645=DIRECTION('center_axis',(0.,0.,1.));
#4646=DIRECTION('ref_axis',(1.,0.,0.));
#4647=DIRECTION('center_axis',(0.,0.,1.));
#4648=DIRECTION('ref_axis',(1.,0.,0.));
#4649=DIRECTION('center_axis',(0.,0.,1.));
#4650=DIRECTION('ref_axis',(1.,0.,0.));
#4651=DIRECTION('center_axis',(0.,1.,0.));
#4652=DIRECTION('ref_axis',(-1.,0.,0.));
#4653=DIRECTION('',(-1.,0.,0.));
#4654=DIRECTION('',(0.,0.,1.));
#4655=DIRECTION('',(-1.,0.,0.));
#4656=DIRECTION('',(0.,0.,1.));
#4657=DIRECTION('center_axis',(-0.866025403784438,0.500000000000001,0.));
#4658=DIRECTION('ref_axis',(-0.500000000000001,-0.866025403784438,0.));
#4659=DIRECTION('',(-0.500000000000001,-0.866025403784438,0.));
#4660=DIRECTION('',(-0.500000000000001,-0.866025403784438,0.));
#4661=DIRECTION('',(0.,0.,1.));
#4662=DIRECTION('center_axis',(-0.866025403784439,-0.5,0.));
#4663=DIRECTION('ref_axis',(0.5,-0.866025403784439,0.));
#4664=DIRECTION('',(0.5,-0.866025403784439,0.));
#4665=DIRECTION('',(0.5,-0.866025403784439,0.));
#4666=DIRECTION('',(0.,0.,1.));
#4667=DIRECTION('center_axis',(0.,-1.,0.));
#4668=DIRECTION('ref_axis',(1.,0.,0.));
#4669=DIRECTION('',(1.,0.,0.));
#4670=DIRECTION('',(1.,0.,0.));
#4671=DIRECTION('',(0.,0.,1.));
#4672=DIRECTION('center_axis',(0.866025403784439,0.5,0.));
#4673=DIRECTION('ref_axis',(-0.5,0.866025403784439,0.));
#4674=DIRECTION('',(-0.5,0.866025403784439,0.));
#4675=DIRECTION('',(0.,0.,1.));
#4676=DIRECTION('',(-0.5,0.866025403784439,0.));
#4677=DIRECTION('center_axis',(0.866025403784439,-0.5,0.));
#4678=DIRECTION('ref_axis',(0.5,0.866025403784439,0.));
#4679=DIRECTION('',(0.5,0.866025403784439,0.));
#4680=DIRECTION('',(0.5,0.866025403784439,0.));
#4681=DIRECTION('center_axis',(0.,0.,1.));
#4682=DIRECTION('ref_axis',(1.,0.,0.));
#4683=DIRECTION('center_axis',(0.,0.,-1.));
#4684=DIRECTION('ref_axis',(1.,0.,0.));
#4685=DIRECTION('center_axis',(0.,0.,1.));
#4686=DIRECTION('ref_axis',(1.,0.,0.));
#4687=DIRECTION('',(0.,0.,-1.));
#4688=DIRECTION('center_axis',(0.,0.,1.));
#4689=DIRECTION('ref_axis',(1.,0.,0.));
#4690=DIRECTION('',(0.,0.,1.));
#4691=DIRECTION('',(1.,0.,0.));
#4692=DIRECTION('',(0.,0.,1.));
#4693=DIRECTION('',(1.,0.,0.));
#4694=DIRECTION('',(0.,0.,1.));
#4695=DIRECTION('',(1.,0.,0.));
#4696=DIRECTION('',(0.,0.,1.));
#4697=DIRECTION('',(1.,0.,0.));
#4698=DIRECTION('',(0.,-1.,2.22044604925031E-16));
#4699=DIRECTION('',(1.,0.,0.));
#4700=DIRECTION('',(0.,-1.,2.22044604925031E-16));
#4701=DIRECTION('',(1.,0.,0.));
#4702=DIRECTION('',(0.,0.,1.));
#4703=DIRECTION('',(1.,0.,0.));
#4704=DIRECTION('',(0.,0.,1.));
#4705=DIRECTION('',(1.,0.,0.));
#4706=DIRECTION('',(0.,-1.,2.22044604925031E-16));
#4707=DIRECTION('',(1.,0.,0.));
#4708=DIRECTION('',(0.,-1.,2.22044604925031E-16));
#4709=DIRECTION('',(1.,0.,0.));
#4710=DIRECTION('',(0.,0.,1.));
#4711=DIRECTION('',(1.,0.,0.));
#4712=DIRECTION('',(0.,0.,1.));
#4713=DIRECTION('',(1.,0.,0.));
#4714=DIRECTION('',(0.,0.,1.));
#4715=DIRECTION('',(1.,0.,0.));
#4716=DIRECTION('',(0.,-1.,2.22044604925031E-16));
#4717=DIRECTION('',(1.,0.,0.));
#4718=DIRECTION('',(0.,-1.,2.22044604925031E-16));
#4719=DIRECTION('',(1.,0.,0.));
#4720=DIRECTION('',(0.,0.,1.));
#4721=DIRECTION('',(1.,0.,0.));
#4722=DIRECTION('',(0.,-1.,2.22044604925031E-16));
#4723=DIRECTION('',(1.,0.,0.));
#4724=DIRECTION('',(0.,-1.,2.22044604925031E-16));
#4725=DIRECTION('',(1.,0.,0.));
#4726=DIRECTION('',(0.,-1.,2.22044604925031E-16));
#4727=DIRECTION('',(1.,0.,0.));
#4728=DIRECTION('',(0.,-1.,2.22044604925031E-16));
#4729=DIRECTION('',(1.,0.,0.));
#4730=DIRECTION('',(0.,0.,1.));
#4731=DIRECTION('',(1.,0.,0.));
#4732=DIRECTION('',(0.,-1.,2.22044604925031E-16));
#4733=DIRECTION('',(1.,0.,0.));
#4734=DIRECTION('',(0.,-1.,2.22044604925031E-16));
#4735=DIRECTION('',(1.,0.,0.));
#4736=DIRECTION('',(0.,-1.,2.22044604925031E-16));
#4737=DIRECTION('',(1.,0.,0.));
#4738=DIRECTION('',(0.,-1.,2.22044604925031E-16));
#4739=DIRECTION('',(1.,0.,0.));
#4740=DIRECTION('',(-6.88476015422318E-16,2.46519032881566E-32,1.));
#4741=DIRECTION('',(0.989071388633229,-0.147437404301407,3.73446748617153E-16));
#4742=CARTESIAN_POINT('',(0.,0.,0.));
#4743=CARTESIAN_POINT('',(0.,0.,0.));
#4744=CARTESIAN_POINT('Origin',(9.5,-0.3,0.7));
#4745=CARTESIAN_POINT('',(11.5,-0.3,1.));
#4746=CARTESIAN_POINT('',(9.5,-0.3,1.));
#4747=CARTESIAN_POINT('',(8.5,-0.3,1.));
#4748=CARTESIAN_POINT('',(11.5,-0.3,0.7));
#4749=CARTESIAN_POINT('',(11.5,-0.3,0.7));
#4750=CARTESIAN_POINT('',(9.5,-0.3,0.7));
#4751=CARTESIAN_POINT('',(9.5,-0.3,0.7));
#4752=CARTESIAN_POINT('',(9.5,-0.3,0.7));
#4753=CARTESIAN_POINT('Origin',(9.5,0.3,0.7));
#4754=CARTESIAN_POINT('',(9.5,0.3,1.));
#4755=CARTESIAN_POINT('',(9.5,0.15,1.));
#4756=CARTESIAN_POINT('',(9.5,0.3,0.7));
#4757=CARTESIAN_POINT('',(9.5,0.3,0.7));
#4758=CARTESIAN_POINT('',(9.5,0.3,0.7));
#4759=CARTESIAN_POINT('Origin',(11.5,0.3,0.7));
#4760=CARTESIAN_POINT('',(11.5,0.3,1.));
#4761=CARTESIAN_POINT('',(9.5,0.3,1.));
#4762=CARTESIAN_POINT('',(11.5,0.3,0.7));
#4763=CARTESIAN_POINT('',(11.5,0.3,0.7));
#4764=CARTESIAN_POINT('',(11.5,0.3,0.7));
#4765=CARTESIAN_POINT('Origin',(11.5,-0.3,0.7));
#4766=CARTESIAN_POINT('',(11.5,-0.15,1.));
#4767=CARTESIAN_POINT('',(11.5,-0.3,0.7));
#4768=CARTESIAN_POINT('Origin',(10.5,0.,0.7));
#4769=CARTESIAN_POINT('Origin',(3.5,-0.3,0.7));
#4770=CARTESIAN_POINT('',(5.5,-0.3,1.));
#4771=CARTESIAN_POINT('',(3.5,-0.3,1.));
#4772=CARTESIAN_POINT('',(5.5,-0.3,1.));
#4773=CARTESIAN_POINT('',(5.5,-0.3,0.7));
#4774=CARTESIAN_POINT('',(5.5,-0.3,0.7));
#4775=CARTESIAN_POINT('',(3.5,-0.3,0.7));
#4776=CARTESIAN_POINT('',(3.5,-0.3,0.7));
#4777=CARTESIAN_POINT('',(3.5,-0.3,0.7));
#4778=CARTESIAN_POINT('Origin',(3.5,0.3,0.7));
#4779=CARTESIAN_POINT('',(3.5,0.3,1.));
#4780=CARTESIAN_POINT('',(3.5,0.15,1.));
#4781=CARTESIAN_POINT('',(3.5,0.3,0.7));
#4782=CARTESIAN_POINT('',(3.5,0.3,0.7));
#4783=CARTESIAN_POINT('',(3.5,0.3,0.7));
#4784=CARTESIAN_POINT('Origin',(5.5,0.3,0.7));
#4785=CARTESIAN_POINT('',(5.5,0.3,1.));
#4786=CARTESIAN_POINT('',(6.5,0.3,1.));
#4787=CARTESIAN_POINT('',(5.5,0.3,0.7));
#4788=CARTESIAN_POINT('',(5.5,0.3,0.7));
#4789=CARTESIAN_POINT('',(5.5,0.3,0.7));
#4790=CARTESIAN_POINT('Origin',(5.5,-0.3,0.7));
#4791=CARTESIAN_POINT('',(5.5,-0.15,1.));
#4792=CARTESIAN_POINT('',(5.5,-0.3,0.7));
#4793=CARTESIAN_POINT('Origin',(4.5,0.,0.7));
#4794=CARTESIAN_POINT('Origin',(10.5,-2.5,-0.1));
#4795=CARTESIAN_POINT('',(10.25,-2.5,0.));
#4796=CARTESIAN_POINT('Origin',(10.5,-2.5,0.));
#4797=CARTESIAN_POINT('',(10.25,-2.5,1.));
#4798=CARTESIAN_POINT('',(10.25,-2.5,-0.1));
#4799=CARTESIAN_POINT('Origin',(10.5,-2.5,1.));
#4800=CARTESIAN_POINT('Origin',(4.5,2.5,-0.1));
#4801=CARTESIAN_POINT('',(4.25,2.5,0.));
#4802=CARTESIAN_POINT('Origin',(4.5,2.5,0.));
#4803=CARTESIAN_POINT('',(4.25,2.5,1.));
#4804=CARTESIAN_POINT('',(4.25,2.5,-0.1));
#4805=CARTESIAN_POINT('Origin',(4.5,2.5,1.));
#4806=CARTESIAN_POINT('Origin',(4.5,-2.5,-0.1));
#4807=CARTESIAN_POINT('',(4.25,-2.5,0.));
#4808=CARTESIAN_POINT('Origin',(4.5,-2.5,0.));
#4809=CARTESIAN_POINT('',(4.25,-2.5,1.));
#4810=CARTESIAN_POINT('',(4.25,-2.5,-0.1));
#4811=CARTESIAN_POINT('Origin',(4.5,-2.5,1.));
#4812=CARTESIAN_POINT('Origin',(10.5,2.5,-0.1));
#4813=CARTESIAN_POINT('',(10.25,2.5,0.));
#4814=CARTESIAN_POINT('Origin',(10.5,2.5,0.));
#4815=CARTESIAN_POINT('',(10.25,2.5,1.));
#4816=CARTESIAN_POINT('',(10.25,2.5,-0.1));
#4817=CARTESIAN_POINT('Origin',(10.5,2.5,1.));
#4818=CARTESIAN_POINT('Origin',(7.5,-4.,-0.1));
#4819=CARTESIAN_POINT('',(7.16,-4.,0.));
#4820=CARTESIAN_POINT('Origin',(7.5,-4.,0.));
#4821=CARTESIAN_POINT('',(7.16,-4.,1.));
#4822=CARTESIAN_POINT('',(7.16,-4.,-0.1));
#4823=CARTESIAN_POINT('Origin',(7.5,-4.,1.));
#4824=CARTESIAN_POINT('Origin',(7.5,4.,-0.1));
#4825=CARTESIAN_POINT('',(7.16,4.,0.));
#4826=CARTESIAN_POINT('Origin',(7.5,4.,0.));
#4827=CARTESIAN_POINT('',(7.16,4.,1.));
#4828=CARTESIAN_POINT('',(7.16,4.,-0.1));
#4829=CARTESIAN_POINT('Origin',(7.5,4.,1.));
#4830=CARTESIAN_POINT('Origin',(12.5,2.5,-0.1));
#4831=CARTESIAN_POINT('',(12.16,2.5,0.));
#4832=CARTESIAN_POINT('Origin',(12.5,2.5,0.));
#4833=CARTESIAN_POINT('',(12.16,2.5,1.));
#4834=CARTESIAN_POINT('',(12.16,2.5,-0.1));
#4835=CARTESIAN_POINT('Origin',(12.5,2.5,1.));
#4836=CARTESIAN_POINT('Origin',(12.5,-2.5,-0.1));
#4837=CARTESIAN_POINT('',(12.16,-2.5,0.));
#4838=CARTESIAN_POINT('Origin',(12.5,-2.5,0.));
#4839=CARTESIAN_POINT('',(12.16,-2.5,1.));
#4840=CARTESIAN_POINT('',(12.16,-2.5,-0.1));
#4841=CARTESIAN_POINT('Origin',(12.5,-2.5,1.));
#4842=CARTESIAN_POINT('Origin',(10.,5.,-0.1));
#4843=CARTESIAN_POINT('',(9.66,5.,0.));
#4844=CARTESIAN_POINT('Origin',(10.,5.,0.));
#4845=CARTESIAN_POINT('',(9.66,5.,1.));
#4846=CARTESIAN_POINT('',(9.66,5.,-0.1));
#4847=CARTESIAN_POINT('Origin',(10.,5.,1.));
#4848=CARTESIAN_POINT('Origin',(7.5,5.,-0.1));
#4849=CARTESIAN_POINT('',(7.16,5.,0.));
#4850=CARTESIAN_POINT('Origin',(7.5,5.,0.));
#4851=CARTESIAN_POINT('',(7.16,5.,1.));
#4852=CARTESIAN_POINT('',(7.16,5.,-0.1));
#4853=CARTESIAN_POINT('Origin',(7.5,5.,1.));
#4854=CARTESIAN_POINT('Origin',(2.5,-5.,-0.1));
#4855=CARTESIAN_POINT('',(2.16,-5.,0.));
#4856=CARTESIAN_POINT('Origin',(2.5,-5.,0.));
#4857=CARTESIAN_POINT('',(2.16,-5.,1.));
#4858=CARTESIAN_POINT('',(2.16,-5.,-0.1));
#4859=CARTESIAN_POINT('Origin',(2.5,-5.,1.));
#4860=CARTESIAN_POINT('Origin',(7.5,-2.5,-0.1));
#4861=CARTESIAN_POINT('',(7.16,-2.5,0.));
#4862=CARTESIAN_POINT('Origin',(7.5,-2.5,0.));
#4863=CARTESIAN_POINT('',(7.16,-2.5,1.));
#4864=CARTESIAN_POINT('',(7.16,-2.5,-0.1));
#4865=CARTESIAN_POINT('Origin',(7.5,-2.5,1.));
#4866=CARTESIAN_POINT('Origin',(5.,5.,-0.1));
#4867=CARTESIAN_POINT('',(4.66,5.,0.));
#4868=CARTESIAN_POINT('Origin',(5.,5.,0.));
#4869=CARTESIAN_POINT('',(4.66,5.,1.));
#4870=CARTESIAN_POINT('',(4.66,5.,-0.1));
#4871=CARTESIAN_POINT('Origin',(5.,5.,1.));
#4872=CARTESIAN_POINT('Origin',(2.5,5.,-0.1));
#4873=CARTESIAN_POINT('',(2.16,5.,0.));
#4874=CARTESIAN_POINT('Origin',(2.5,5.,0.));
#4875=CARTESIAN_POINT('',(2.16,5.,1.));
#4876=CARTESIAN_POINT('',(2.16,5.,-0.1));
#4877=CARTESIAN_POINT('Origin',(2.5,5.,1.));
#4878=CARTESIAN_POINT('Origin',(2.5,0.,-0.1));
#4879=CARTESIAN_POINT('',(2.16,-4.163799117101E-17,0.));
#4880=CARTESIAN_POINT('Origin',(2.5,0.,0.));
#4881=CARTESIAN_POINT('',(2.16,4.163799117101E-17,1.));
#4882=CARTESIAN_POINT('',(2.16,-4.163799117101E-17,-0.1));
#4883=CARTESIAN_POINT('Origin',(2.5,0.,1.));
#4884=CARTESIAN_POINT('Origin',(2.5,-2.5,-0.1));
#4885=CARTESIAN_POINT('',(2.16,-2.5,0.));
#4886=CARTESIAN_POINT('Origin',(2.5,-2.5,0.));
#4887=CARTESIAN_POINT('',(2.16,-2.5,1.));
#4888=CARTESIAN_POINT('',(2.16,-2.5,-0.1));
#4889=CARTESIAN_POINT('Origin',(2.5,-2.5,1.));
#4890=CARTESIAN_POINT('Origin',(2.5,2.5,-0.1));
#4891=CARTESIAN_POINT('',(2.16,2.5,0.));
#4892=CARTESIAN_POINT('Origin',(2.5,2.5,0.));
#4893=CARTESIAN_POINT('',(2.16,2.5,1.));
#4894=CARTESIAN_POINT('',(2.16,2.5,-0.1));
#4895=CARTESIAN_POINT('Origin',(2.5,2.5,1.));
#4896=CARTESIAN_POINT('Origin',(5.,-5.,-0.1));
#4897=CARTESIAN_POINT('',(4.66,-5.,0.));
#4898=CARTESIAN_POINT('Origin',(5.,-5.,0.));
#4899=CARTESIAN_POINT('',(4.66,-5.,1.));
#4900=CARTESIAN_POINT('',(4.66,-5.,-0.1));
#4901=CARTESIAN_POINT('Origin',(5.,-5.,1.));
#4902=CARTESIAN_POINT('Origin',(7.5,-5.,-0.1));
#4903=CARTESIAN_POINT('',(7.16,-5.,0.));
#4904=CARTESIAN_POINT('Origin',(7.5,-5.,0.));
#4905=CARTESIAN_POINT('',(7.16,-5.,1.));
#4906=CARTESIAN_POINT('',(7.16,-5.,-0.1));
#4907=CARTESIAN_POINT('Origin',(7.5,-5.,1.));
#4908=CARTESIAN_POINT('Origin',(7.5,0.,-0.1));
#4909=CARTESIAN_POINT('',(7.16,-4.163799117101E-17,0.));
#4910=CARTESIAN_POINT('Origin',(7.5,0.,0.));
#4911=CARTESIAN_POINT('',(7.16,4.163799117101E-17,1.));
#4912=CARTESIAN_POINT('',(7.16,-4.163799117101E-17,-0.1));
#4913=CARTESIAN_POINT('Origin',(7.5,0.,1.));
#4914=CARTESIAN_POINT('Origin',(7.5,2.5,-0.1));
#4915=CARTESIAN_POINT('',(7.16,2.5,0.));
#4916=CARTESIAN_POINT('Origin',(7.5,2.5,0.));
#4917=CARTESIAN_POINT('',(7.16,2.5,1.));
#4918=CARTESIAN_POINT('',(7.16,2.5,-0.1));
#4919=CARTESIAN_POINT('Origin',(7.5,2.5,1.));
#4920=CARTESIAN_POINT('Origin',(10.,-5.,-0.1));
#4921=CARTESIAN_POINT('',(9.66,-5.,0.));
#4922=CARTESIAN_POINT('Origin',(10.,-5.,0.));
#4923=CARTESIAN_POINT('',(9.66,-5.,1.));
#4924=CARTESIAN_POINT('',(9.66,-5.,-0.1));
#4925=CARTESIAN_POINT('Origin',(10.,-5.,1.));
#4926=CARTESIAN_POINT('Origin',(12.5,-5.,-0.1));
#4927=CARTESIAN_POINT('',(12.16,-5.,0.));
#4928=CARTESIAN_POINT('Origin',(12.5,-5.,0.));
#4929=CARTESIAN_POINT('',(12.16,-5.,1.));
#4930=CARTESIAN_POINT('',(12.16,-5.,-0.1));
#4931=CARTESIAN_POINT('Origin',(12.5,-5.,1.));
#4932=CARTESIAN_POINT('Origin',(12.5,0.,-0.1));
#4933=CARTESIAN_POINT('',(12.16,-4.163799117101E-17,0.));
#4934=CARTESIAN_POINT('Origin',(12.5,0.,0.));
#4935=CARTESIAN_POINT('',(12.16,4.163799117101E-17,1.));
#4936=CARTESIAN_POINT('',(12.16,-4.163799117101E-17,-0.1));
#4937=CARTESIAN_POINT('Origin',(12.5,0.,1.));
#4938=CARTESIAN_POINT('Origin',(12.5,5.,-0.1));
#4939=CARTESIAN_POINT('',(12.16,5.,0.));
#4940=CARTESIAN_POINT('Origin',(12.5,5.,0.));
#4941=CARTESIAN_POINT('',(12.16,5.,1.));
#4942=CARTESIAN_POINT('',(12.16,5.,-0.1));
#4943=CARTESIAN_POINT('Origin',(12.5,5.,1.));
#4944=CARTESIAN_POINT('Origin',(15.,7.5,0.));
#4945=CARTESIAN_POINT('',(15.,7.5,0.));
#4946=CARTESIAN_POINT('',(0.,7.5,0.));
#4947=CARTESIAN_POINT('',(15.,7.5,0.));
#4948=CARTESIAN_POINT('',(0.,7.5,1.));
#4949=CARTESIAN_POINT('',(0.,7.5,0.));
#4950=CARTESIAN_POINT('',(15.,7.5,1.));
#4951=CARTESIAN_POINT('',(15.,7.5,1.));
#4952=CARTESIAN_POINT('',(15.,7.5,0.));
#4953=CARTESIAN_POINT('Origin',(15.,-7.5,0.));
#4954=CARTESIAN_POINT('',(15.,-7.5,0.));
#4955=CARTESIAN_POINT('',(15.,-7.5,0.));
#4956=CARTESIAN_POINT('',(15.,-7.5,1.));
#4957=CARTESIAN_POINT('',(15.,-7.5,1.));
#4958=CARTESIAN_POINT('',(15.,-7.5,0.));
#4959=CARTESIAN_POINT('Origin',(0.,-7.5,0.));
#4960=CARTESIAN_POINT('',(0.,-7.5,0.));
#4961=CARTESIAN_POINT('',(0.,-7.5,0.));
#4962=CARTESIAN_POINT('',(0.,-7.5,1.));
#4963=CARTESIAN_POINT('',(0.,-7.5,1.));
#4964=CARTESIAN_POINT('',(0.,-7.5,0.));
#4965=CARTESIAN_POINT('Origin',(0.,7.5,0.));
#4966=CARTESIAN_POINT('',(0.,7.5,0.));
#4967=CARTESIAN_POINT('',(0.,7.5,1.));
#4968=CARTESIAN_POINT('Origin',(7.5,0.,1.));
#4969=CARTESIAN_POINT('Origin',(7.5,0.,0.));
#4970=CARTESIAN_POINT('',(0.,0.,0.));
#4971=CARTESIAN_POINT('Origin',(-1.,0.,0.35));
#4972=CARTESIAN_POINT('',(-1.,-0.26,0.6));
#4973=CARTESIAN_POINT('',(-1.,-0.3,0.56));
#4974=CARTESIAN_POINT('',(-1.,-0.2675,0.5925));
#4975=CARTESIAN_POINT('',(-1.,0.26,0.6));
#4976=CARTESIAN_POINT('',(-1.,0.,0.6));
#4977=CARTESIAN_POINT('',(-1.,0.3,0.56));
#4978=CARTESIAN_POINT('',(-1.,0.2675,0.5925));
#4979=CARTESIAN_POINT('',(-1.,0.3,0.04));
#4980=CARTESIAN_POINT('',(-1.,0.3,0.175));
#4981=CARTESIAN_POINT('',(-1.,0.26,0.));
#4982=CARTESIAN_POINT('',(-1.,0.2925,0.0325));
#4983=CARTESIAN_POINT('',(-1.,-0.26,0.));
#4984=CARTESIAN_POINT('',(-1.,0.,0.));
#4985=CARTESIAN_POINT('',(-1.,-0.3,0.04));
#4986=CARTESIAN_POINT('',(-1.,-0.2925,0.0325));
#4987=CARTESIAN_POINT('',(-1.,-0.3,0.175));
#4988=CARTESIAN_POINT('Origin',(0.75,0.28,0.02));
#4989=CARTESIAN_POINT('',(1.,0.3,0.04));
#4990=CARTESIAN_POINT('',(0.75,0.3,0.04));
#4991=CARTESIAN_POINT('',(1.,0.26,0.));
#4992=CARTESIAN_POINT('',(1.,0.2925,0.0325));
#4993=CARTESIAN_POINT('',(0.75,0.26,0.));
#4994=CARTESIAN_POINT('Origin',(1.5,0.3,0.));
#4995=CARTESIAN_POINT('',(1.,0.3,0.56));
#4996=CARTESIAN_POINT('',(0.75,0.3,0.56));
#4997=CARTESIAN_POINT('',(1.,0.3,0.175));
#4998=CARTESIAN_POINT('Origin',(0.75,0.28,0.58));
#4999=CARTESIAN_POINT('',(1.,0.26,0.6));
#5000=CARTESIAN_POINT('',(0.75,0.26,0.6));
#5001=CARTESIAN_POINT('',(1.,0.2675,0.5925));
#5002=CARTESIAN_POINT('Origin',(0.,0.,0.6));
#5003=CARTESIAN_POINT('',(1.,-0.26,0.6));
#5004=CARTESIAN_POINT('',(-0.75,-0.26,0.6));
#5005=CARTESIAN_POINT('',(1.,0.,0.6));
#5006=CARTESIAN_POINT('Origin',(1.,0.,0.35));
#5007=CARTESIAN_POINT('',(1.,-0.26,0.));
#5008=CARTESIAN_POINT('',(1.,-0.3,0.04));
#5009=CARTESIAN_POINT('',(1.,-0.2925,0.0325));
#5010=CARTESIAN_POINT('',(1.,0.,0.));
#5011=CARTESIAN_POINT('',(1.,-0.3,0.56));
#5012=CARTESIAN_POINT('',(1.,-0.2675,0.5925));
#5013=CARTESIAN_POINT('',(1.,-0.3,0.175));
#5014=CARTESIAN_POINT('Origin',(0.,0.,0.));
#5015=CARTESIAN_POINT('',(-0.75,-0.26,0.));
#5016=CARTESIAN_POINT('Origin',(-0.75,-0.28,0.58));
#5017=CARTESIAN_POINT('',(-0.75,-0.3,0.56));
#5018=CARTESIAN_POINT('Origin',(-0.75,-0.28,0.02));
#5019=CARTESIAN_POINT('',(-0.75,-0.3,0.04));
#5020=CARTESIAN_POINT('Origin',(-1.5,-0.3,0.));
#5021=CARTESIAN_POINT('',(0.,0.,0.));
#5022=CARTESIAN_POINT('Origin',(6.5,2.5,2.5));
#5023=CARTESIAN_POINT('',(6.,2.5,2.5));
#5024=CARTESIAN_POINT('',(6.,2.5,5.));
#5025=CARTESIAN_POINT('',(6.,2.5,2.5));
#5026=CARTESIAN_POINT('',(6.5,3.,2.5));
#5027=CARTESIAN_POINT('Origin',(6.5,2.5,2.5));
#5028=CARTESIAN_POINT('',(6.5,3.,5.));
#5029=CARTESIAN_POINT('',(6.5,3.,2.5));
#5030=CARTESIAN_POINT('Origin',(6.5,2.5,5.));
#5031=CARTESIAN_POINT('Origin',(6.5,-2.5,2.5));
#5032=CARTESIAN_POINT('',(6.,-2.5,2.5));
#5033=CARTESIAN_POINT('',(6.,-2.5,5.));
#5034=CARTESIAN_POINT('',(6.,-2.5,2.5));
#5035=CARTESIAN_POINT('',(6.5,-3.,2.5));
#5036=CARTESIAN_POINT('Origin',(6.5,-2.5,2.5));
#5037=CARTESIAN_POINT('',(6.5,-3.,5.));
#5038=CARTESIAN_POINT('',(6.5,-3.,2.5));
#5039=CARTESIAN_POINT('',(7.,-2.5,5.));
#5040=CARTESIAN_POINT('Origin',(6.5,-2.5,5.));
#5041=CARTESIAN_POINT('Origin',(6.5,-2.5,5.));
#5042=CARTESIAN_POINT('Origin',(5.5,-0.3,0.9));
#5043=CARTESIAN_POINT('',(5.5,-0.3,1.));
#5044=CARTESIAN_POINT('',(7.5,-0.3,1.));
#5045=CARTESIAN_POINT('',(6.,-0.3,1.));
#5046=CARTESIAN_POINT('',(5.5,-0.3,1.3));
#5047=CARTESIAN_POINT('',(5.5,-0.3,0.9));
#5048=CARTESIAN_POINT('',(7.5,-0.3,1.3));
#5049=CARTESIAN_POINT('',(5.5,-0.3,1.3));
#5050=CARTESIAN_POINT('',(7.5,-0.3,0.9));
#5051=CARTESIAN_POINT('Origin',(7.5,-0.3,0.9));
#5052=CARTESIAN_POINT('',(7.5,0.3,1.));
#5053=CARTESIAN_POINT('',(7.5,-0.15,1.));
#5054=CARTESIAN_POINT('',(7.5,0.3,1.3));
#5055=CARTESIAN_POINT('',(7.5,-0.3,1.3));
#5056=CARTESIAN_POINT('',(7.5,0.3,0.9));
#5057=CARTESIAN_POINT('Origin',(7.5,0.3,0.9));
#5058=CARTESIAN_POINT('',(5.5,0.3,1.));
#5059=CARTESIAN_POINT('',(7.,0.3,1.));
#5060=CARTESIAN_POINT('',(5.5,0.3,1.3));
#5061=CARTESIAN_POINT('',(7.5,0.3,1.3));
#5062=CARTESIAN_POINT('',(5.5,0.3,0.9));
#5063=CARTESIAN_POINT('Origin',(5.5,0.3,0.9));
#5064=CARTESIAN_POINT('',(5.5,0.15,1.));
#5065=CARTESIAN_POINT('',(5.5,0.3,1.3));
#5066=CARTESIAN_POINT('Origin',(6.5,0.,1.3));
#5067=CARTESIAN_POINT('Origin',(6.5,-2.5,2.5));
#5068=CARTESIAN_POINT('Origin',(6.5,-2.5,5.));
#5069=CARTESIAN_POINT('',(6.5,-3.,2.5));
#5070=CARTESIAN_POINT('Origin',(6.5,-2.5,2.5));
#5071=CARTESIAN_POINT('Origin',(6.5,-2.5,2.5));
#5072=CARTESIAN_POINT('',(6.17,-2.5,2.5));
#5073=CARTESIAN_POINT('Origin',(6.5,-2.5,2.5));
#5074=CARTESIAN_POINT('Origin',(6.5,2.5,2.5));
#5075=CARTESIAN_POINT('',(7.,2.5,5.));
#5076=CARTESIAN_POINT('Origin',(6.5,2.5,5.));
#5077=CARTESIAN_POINT('Origin',(6.5,2.5,5.));
#5078=CARTESIAN_POINT('',(6.5,3.,2.5));
#5079=CARTESIAN_POINT('Origin',(6.5,2.5,2.5));
#5080=CARTESIAN_POINT('Origin',(6.5,2.5,2.5));
#5081=CARTESIAN_POINT('',(6.17,2.5,2.5));
#5082=CARTESIAN_POINT('Origin',(6.5,2.5,2.5));
#5083=CARTESIAN_POINT('Origin',(4.9,-2.6,5.1));
#5084=CARTESIAN_POINT('',(8.,-2.5,5.));
#5085=CARTESIAN_POINT('',(5.7,-2.5,5.));
#5086=CARTESIAN_POINT('',(8.,0.,2.5));
#5087=CARTESIAN_POINT('',(8.,-1.675,4.175));
#5088=CARTESIAN_POINT('',(5.,0.,2.5));
#5089=CARTESIAN_POINT('',(4.9,0.,2.5));
#5090=CARTESIAN_POINT('',(5.,-2.5,5.));
#5091=CARTESIAN_POINT('',(5.,-0.175,2.675));
#5092=CARTESIAN_POINT('',(5.7,-2.5,5.));
#5093=CARTESIAN_POINT('Origin',(6.5,0.,5.));
#5094=CARTESIAN_POINT('',(8.,-3.,5.));
#5095=CARTESIAN_POINT('',(5.,-3.,5.));
#5096=CARTESIAN_POINT('',(8.,-3.,5.));
#5097=CARTESIAN_POINT('Origin',(4.9,0.,2.5));
#5098=CARTESIAN_POINT('',(5.,2.5,5.));
#5099=CARTESIAN_POINT('',(5.7,2.5,5.));
#5100=CARTESIAN_POINT('',(5.,0.375,2.875));
#5101=CARTESIAN_POINT('',(8.,2.5,5.));
#5102=CARTESIAN_POINT('',(8.,-1.125,1.375));
#5103=CARTESIAN_POINT('',(5.7,2.5,5.));
#5104=CARTESIAN_POINT('Origin',(6.5,0.,5.));
#5105=CARTESIAN_POINT('',(5.,3.,5.));
#5106=CARTESIAN_POINT('',(8.,3.,5.));
#5107=CARTESIAN_POINT('',(5.,3.,5.));
#5108=CARTESIAN_POINT('Origin',(6.5,-2.5,0.9));
#5109=CARTESIAN_POINT('',(6.17,-2.5,1.));
#5110=CARTESIAN_POINT('Origin',(6.5,-2.5,1.));
#5111=CARTESIAN_POINT('',(6.17,-2.5,0.9));
#5112=CARTESIAN_POINT('Origin',(6.5,2.5,0.9));
#5113=CARTESIAN_POINT('',(6.17,2.5,1.));
#5114=CARTESIAN_POINT('Origin',(6.5,2.5,1.));
#5115=CARTESIAN_POINT('',(6.17,2.5,0.9));
#5116=CARTESIAN_POINT('Origin',(6.5,0.,5.));
#5117=CARTESIAN_POINT('',(5.,-3.,5.));
#5118=CARTESIAN_POINT('',(5.,3.,5.));
#5119=CARTESIAN_POINT('',(5.,-3.,5.));
#5120=CARTESIAN_POINT('Origin',(6.5,0.,5.));
#5121=CARTESIAN_POINT('',(8.,3.,5.));
#5122=CARTESIAN_POINT('',(8.,-3.,5.));
#5123=CARTESIAN_POINT('',(8.,3.,5.));
#5124=CARTESIAN_POINT('Origin',(5.,3.,1.));
#5125=CARTESIAN_POINT('',(5.,3.,1.));
#5126=CARTESIAN_POINT('',(5.,3.,1.));
#5127=CARTESIAN_POINT('',(5.,-3.,1.));
#5128=CARTESIAN_POINT('',(5.,3.,1.));
#5129=CARTESIAN_POINT('',(5.,-3.,1.));
#5130=CARTESIAN_POINT('Origin',(8.,3.,1.));
#5131=CARTESIAN_POINT('',(8.,3.,1.));
#5132=CARTESIAN_POINT('',(8.,3.,1.));
#5133=CARTESIAN_POINT('',(8.,3.,1.));
#5134=CARTESIAN_POINT('Origin',(8.,-3.,1.));
#5135=CARTESIAN_POINT('',(8.,-3.,1.));
#5136=CARTESIAN_POINT('',(8.,-3.,1.));
#5137=CARTESIAN_POINT('',(8.,-3.,1.));
#5138=CARTESIAN_POINT('Origin',(5.,-3.,1.));
#5139=CARTESIAN_POINT('',(5.,-3.,1.));
#5140=CARTESIAN_POINT('Origin',(6.5,0.,1.));
#5141=CARTESIAN_POINT('Origin',(8.,-3.,5.));
#5142=CARTESIAN_POINT('',(8.,-3.,5.));
#5143=CARTESIAN_POINT('',(5.,-3.,5.));
#5144=CARTESIAN_POINT('',(8.,-3.,5.));
#5145=CARTESIAN_POINT('',(5.,-3.5,5.));
#5146=CARTESIAN_POINT('',(5.,-3.,5.));
#5147=CARTESIAN_POINT('',(8.,-3.5,5.));
#5148=CARTESIAN_POINT('',(8.,-3.5,5.));
#5149=CARTESIAN_POINT('',(8.,-3.,5.));
#5150=CARTESIAN_POINT('Origin',(8.,-3.,1.));
#5151=CARTESIAN_POINT('',(8.,-3.,1.));
#5152=CARTESIAN_POINT('',(8.,-3.,1.));
#5153=CARTESIAN_POINT('',(8.,-3.5,1.));
#5154=CARTESIAN_POINT('',(8.,-3.5,1.));
#5155=CARTESIAN_POINT('',(8.,-3.,1.));
#5156=CARTESIAN_POINT('Origin',(5.,-3.,1.));
#5157=CARTESIAN_POINT('',(5.,-3.,1.));
#5158=CARTESIAN_POINT('',(5.,-3.,1.));
#5159=CARTESIAN_POINT('',(5.,-3.5,1.));
#5160=CARTESIAN_POINT('',(5.,-3.5,1.));
#5161=CARTESIAN_POINT('',(5.,-3.,1.));
#5162=CARTESIAN_POINT('Origin',(5.,-3.,5.));
#5163=CARTESIAN_POINT('',(5.,-3.,5.));
#5164=CARTESIAN_POINT('',(5.,-3.5,5.));
#5165=CARTESIAN_POINT('Origin',(6.5,-3.5,3.));
#5166=CARTESIAN_POINT('Origin',(6.5,-3.,3.));
#5167=CARTESIAN_POINT('Origin',(5.,3.,5.));
#5168=CARTESIAN_POINT('',(5.,3.,5.));
#5169=CARTESIAN_POINT('',(8.,3.,5.));
#5170=CARTESIAN_POINT('',(5.,3.,5.));
#5171=CARTESIAN_POINT('',(8.,3.5,5.));
#5172=CARTESIAN_POINT('',(8.,3.,5.));
#5173=CARTESIAN_POINT('',(5.,3.5,5.));
#5174=CARTESIAN_POINT('',(5.,3.5,5.));
#5175=CARTESIAN_POINT('',(5.,3.,5.));
#5176=CARTESIAN_POINT('Origin',(5.,3.,1.));
#5177=CARTESIAN_POINT('',(5.,3.,1.));
#5178=CARTESIAN_POINT('',(5.,3.,1.));
#5179=CARTESIAN_POINT('',(5.,3.5,1.));
#5180=CARTESIAN_POINT('',(5.,3.5,1.));
#5181=CARTESIAN_POINT('',(5.,3.,1.));
#5182=CARTESIAN_POINT('Origin',(8.,3.,1.));
#5183=CARTESIAN_POINT('',(8.,3.,1.));
#5184=CARTESIAN_POINT('',(8.,3.,1.));
#5185=CARTESIAN_POINT('',(8.,3.5,1.));
#5186=CARTESIAN_POINT('',(8.,3.5,1.));
#5187=CARTESIAN_POINT('',(8.,3.,1.));
#5188=CARTESIAN_POINT('Origin',(8.,3.,5.));
#5189=CARTESIAN_POINT('',(8.,3.,5.));
#5190=CARTESIAN_POINT('',(8.,3.5,5.));
#5191=CARTESIAN_POINT('Origin',(6.5,3.5,3.));
#5192=CARTESIAN_POINT('Origin',(6.5,3.,3.));
#5193=CARTESIAN_POINT('',(0.,0.,0.));
#5194=CARTESIAN_POINT('Origin',(0.45,0.6,0.));
#5195=CARTESIAN_POINT('',(-0.45,0.6,-5.51091059616309E-17));
#5196=CARTESIAN_POINT('Origin',(0.,0.6,0.));
#5197=CARTESIAN_POINT('Origin',(0.,0.575,0.));
#5198=CARTESIAN_POINT('',(-0.5,0.55,-6.12323399573677E-17));
#5199=CARTESIAN_POINT('Origin',(0.,0.55,0.));
#5200=CARTESIAN_POINT('',(-0.475,0.575,-5.81707229594993E-17));
#5201=CARTESIAN_POINT('Origin',(0.,0.29,0.));
#5202=CARTESIAN_POINT('',(-0.5,0.0299999999999998,-6.12323399573677E-17));
#5203=CARTESIAN_POINT('Origin',(0.,0.0299999999999998,0.));
#5204=CARTESIAN_POINT('',(-0.5,0.29,-6.12323399573677E-17));
#5205=CARTESIAN_POINT('Origin',(0.,0.0150000000000001,0.));
#5206=CARTESIAN_POINT('',(-0.47,7.11236625150491E-17,-5.75583995599256E-17));
#5207=CARTESIAN_POINT('Origin',(0.,0.,0.));
#5208=CARTESIAN_POINT('',(-0.485,0.0150000000000001,-5.93953697586466E-17));
#5209=CARTESIAN_POINT('Origin',(0.32,0.,0.));
#5210=CARTESIAN_POINT('',(-0.32,-6.93889390390723E-18,-3.91886975727153E-17));
#5211=CARTESIAN_POINT('Origin',(0.,0.,0.));
#5212=CARTESIAN_POINT('Origin',(0.,-0.02,0.));
#5213=CARTESIAN_POINT('',(-0.2942,-0.0515999999999999,3.60291088309151E-17));
#5214=CARTESIAN_POINT('Origin',(0.,-0.0515999999999999,0.));
#5215=CARTESIAN_POINT('',(-0.31,-0.02,-3.7964050773568E-17));
#5216=CARTESIAN_POINT('Origin',(0.,-1.24,0.));
#5217=CARTESIAN_POINT('',(-0.2942,-2.4458,3.60291088309151E-17));
#5218=CARTESIAN_POINT('Origin',(0.,-2.4458,0.));
#5219=CARTESIAN_POINT('',(-0.2942,-1.24,-3.60291088309151E-17));
#5220=CARTESIAN_POINT('Origin',(0.,-2.47,0.));
#5221=CARTESIAN_POINT('',(-0.24,-2.5,-2.93915231795365E-17));
#5222=CARTESIAN_POINT('Origin',(0.,-2.5,0.));
#5223=CARTESIAN_POINT('',(-0.27,-2.47,-3.30654635769785E-17));
#5224=CARTESIAN_POINT('Origin',(0.,-2.5,0.));
#5225=CARTESIAN_POINT('Origin',(0.144337567297406,-0.6,-0.25));
#5226=CARTESIAN_POINT('',(0.288675134594813,-0.6,0.));
#5227=CARTESIAN_POINT('',(0.144337567297406,-0.6,-0.25));
#5228=CARTESIAN_POINT('',(0.288675134594813,-0.6,0.));
#5229=CARTESIAN_POINT('',(0.144337567297406,-0.96,-0.25));
#5230=CARTESIAN_POINT('',(0.144337567297406,-0.6,-0.25));
#5231=CARTESIAN_POINT('',(0.288675134594813,-0.96,0.));
#5232=CARTESIAN_POINT('',(0.288675134594813,-0.96,0.));
#5233=CARTESIAN_POINT('',(0.288675134594813,-0.6,0.));
#5234=CARTESIAN_POINT('Origin',(-0.144337567297406,-0.6,-0.25));
#5235=CARTESIAN_POINT('',(-0.144337567297406,-0.6,-0.25));
#5236=CARTESIAN_POINT('',(0.144337567297406,-0.6,-0.25));
#5237=CARTESIAN_POINT('',(-0.144337567297406,-0.96,-0.25));
#5238=CARTESIAN_POINT('',(-0.144337567297406,-0.6,-0.25));
#5239=CARTESIAN_POINT('',(0.144337567297406,-0.96,-0.25));
#5240=CARTESIAN_POINT('Origin',(-0.288675134594813,-0.6,-8.32667268468867E-17));
#5241=CARTESIAN_POINT('',(-0.288675134594813,-0.6,-3.53525079574969E-17));
#5242=CARTESIAN_POINT('',(-0.144337567297406,-0.6,-0.25));
#5243=CARTESIAN_POINT('',(-0.288675134594813,-0.96,-5.55111512312578E-17));
#5244=CARTESIAN_POINT('',(-0.288675134594813,-0.6,-3.53525079574969E-17));
#5245=CARTESIAN_POINT('',(-0.144337567297406,-0.96,-0.25));
#5246=CARTESIAN_POINT('Origin',(-0.144337567297407,-0.6,0.25));
#5247=CARTESIAN_POINT('',(-0.144337567297407,-0.6,0.25));
#5248=CARTESIAN_POINT('',(-0.288675134594813,-0.6,-3.53525079574969E-17));
#5249=CARTESIAN_POINT('',(-0.144337567297407,-0.96,0.25));
#5250=CARTESIAN_POINT('',(-0.144337567297407,-0.6,0.25));
#5251=CARTESIAN_POINT('',(-0.288675134594813,-0.96,-3.53525079574969E-17));
#5252=CARTESIAN_POINT('Origin',(0.144337567297406,-0.6,0.25));
#5253=CARTESIAN_POINT('',(0.144337567297406,-0.6,0.25));
#5254=CARTESIAN_POINT('',(-0.144337567297407,-0.6,0.25));
#5255=CARTESIAN_POINT('',(0.144337567297406,-0.96,0.25));
#5256=CARTESIAN_POINT('',(0.144337567297406,-0.6,0.25));
#5257=CARTESIAN_POINT('',(-0.144337567297407,-0.96,0.25));
#5258=CARTESIAN_POINT('Origin',(0.288675134594813,-0.6,0.));
#5259=CARTESIAN_POINT('',(0.144337567297406,-0.6,0.25));
#5260=CARTESIAN_POINT('',(0.144337567297406,-0.96,0.25));
#5261=CARTESIAN_POINT('Origin',(0.,-0.6,0.));
#5262=CARTESIAN_POINT('Origin',(0.,-0.96,0.));
#5263=CARTESIAN_POINT('',(0.,0.,0.));
#5264=CARTESIAN_POINT('Origin',(10.,-0.8,6.42132034));
#5265=CARTESIAN_POINT('',(9.775,-0.8,6.52132034));
#5266=CARTESIAN_POINT('Origin',(10.,-0.8,6.52132034));
#5267=CARTESIAN_POINT('',(9.775,-0.8,7.12132034));
#5268=CARTESIAN_POINT('',(9.775,-0.8,6.42132034));
#5269=CARTESIAN_POINT('Origin',(10.,-0.8,7.12132034));
#5270=CARTESIAN_POINT('Origin',(10.,0.8,6.42132034));
#5271=CARTESIAN_POINT('',(9.775,0.8,6.52132034));
#5272=CARTESIAN_POINT('Origin',(10.,0.8,6.52132034));
#5273=CARTESIAN_POINT('',(9.775,0.8,7.12132034));
#5274=CARTESIAN_POINT('',(9.775,0.8,6.42132034));
#5275=CARTESIAN_POINT('Origin',(10.,0.8,7.12132034));
#5276=CARTESIAN_POINT('Origin',(10.,-4.,6.42132034));
#5277=CARTESIAN_POINT('',(9.55,-4.,6.52132034));
#5278=CARTESIAN_POINT('Origin',(10.,-4.,6.52132034));
#5279=CARTESIAN_POINT('',(9.55,-4.,7.12132034));
#5280=CARTESIAN_POINT('',(9.55,-4.,6.42132034));
#5281=CARTESIAN_POINT('Origin',(10.,-4.,7.12132034));
#5282=CARTESIAN_POINT('Origin',(10.,4.,6.42132034));
#5283=CARTESIAN_POINT('',(9.55,4.,6.52132034));
#5284=CARTESIAN_POINT('Origin',(10.,4.,6.52132034));
#5285=CARTESIAN_POINT('',(9.55,4.,7.12132034));
#5286=CARTESIAN_POINT('',(9.55,4.,6.42132034));
#5287=CARTESIAN_POINT('Origin',(10.,4.,7.12132034));
#5288=CARTESIAN_POINT('Origin',(11.,4.7,6.52132034));
#5289=CARTESIAN_POINT('',(11.,4.7,6.52132034));
#5290=CARTESIAN_POINT('',(9.,4.7,6.52132034));
#5291=CARTESIAN_POINT('',(11.,4.7,6.52132034));
#5292=CARTESIAN_POINT('',(9.,4.7,7.12132034));
#5293=CARTESIAN_POINT('',(9.,4.7,6.52132034));
#5294=CARTESIAN_POINT('',(11.,4.7,7.12132034));
#5295=CARTESIAN_POINT('',(11.,4.7,7.12132034));
#5296=CARTESIAN_POINT('',(11.,4.7,6.52132034));
#5297=CARTESIAN_POINT('Origin',(11.,-4.7,6.52132034));
#5298=CARTESIAN_POINT('',(11.,-4.7,6.52132034));
#5299=CARTESIAN_POINT('',(11.,-4.7,6.52132034));
#5300=CARTESIAN_POINT('',(11.,-4.7,7.12132034));
#5301=CARTESIAN_POINT('',(11.,-4.7,7.12132034));
#5302=CARTESIAN_POINT('',(11.,-4.7,6.52132034));
#5303=CARTESIAN_POINT('Origin',(9.,-4.7,6.52132034));
#5304=CARTESIAN_POINT('',(9.,-4.7,6.52132034));
#5305=CARTESIAN_POINT('',(9.,-4.7,6.52132034));
#5306=CARTESIAN_POINT('',(9.,-4.7,7.12132034));
#5307=CARTESIAN_POINT('',(9.,-4.7,7.12132034));
#5308=CARTESIAN_POINT('',(9.,-4.7,6.52132034));
#5309=CARTESIAN_POINT('Origin',(9.,4.7,6.52132034));
#5310=CARTESIAN_POINT('',(9.,4.7,6.52132034));
#5311=CARTESIAN_POINT('',(9.,4.7,7.12132034));
#5312=CARTESIAN_POINT('Origin',(10.,0.,7.12132034));
#5313=CARTESIAN_POINT('Origin',(10.,0.,6.52132034));
#5314=CARTESIAN_POINT('',(0.,0.,0.));
#5315=CARTESIAN_POINT('Origin',(10.,-0.8,6.02132034));
#5316=CARTESIAN_POINT('',(9.835,-0.8,6.02132034));
#5317=CARTESIAN_POINT('Origin',(10.,-0.8,6.02132034));
#5318=CARTESIAN_POINT('',(9.835,-0.8,6.52132034));
#5319=CARTESIAN_POINT('',(9.835,-0.8,6.02132034));
#5320=CARTESIAN_POINT('Origin',(10.,-0.8,6.52132034));
#5321=CARTESIAN_POINT('Origin',(10.,-0.8,6.02132034));
#5322=CARTESIAN_POINT('Origin',(10.,0.8,6.02132034));
#5323=CARTESIAN_POINT('',(9.835,0.8,6.02132034));
#5324=CARTESIAN_POINT('Origin',(10.,0.8,6.02132034));
#5325=CARTESIAN_POINT('',(9.835,0.8,6.52132034));
#5326=CARTESIAN_POINT('',(9.835,0.8,6.02132034));
#5327=CARTESIAN_POINT('Origin',(10.,0.8,6.52132034));
#5328=CARTESIAN_POINT('Origin',(10.,0.8,6.02132034));
#5329=CARTESIAN_POINT('Origin',(8.9,0.,4.62132034355964));
#5330=CARTESIAN_POINT('',(11.,1.2,5.52132034));
#5331=CARTESIAN_POINT('',(9.,1.2,5.52132034));
#5332=CARTESIAN_POINT('',(11.,1.2,5.52132034));
#5333=CARTESIAN_POINT('',(11.,-1.2,5.52132034));
#5334=CARTESIAN_POINT('Origin',(11.,0.,4.62132034355964));
#5335=CARTESIAN_POINT('',(9.,-1.2,5.52132034));
#5336=CARTESIAN_POINT('',(9.,-1.2,5.52132034));
#5337=CARTESIAN_POINT('Origin',(9.,0.,4.62132034355964));
#5338=CARTESIAN_POINT('Origin',(11.,-1.2,5.52132034));
#5339=CARTESIAN_POINT('',(11.,1.2,6.52132034));
#5340=CARTESIAN_POINT('',(11.,1.2,5.52132034));
#5341=CARTESIAN_POINT('',(11.,-1.2,6.52132034));
#5342=CARTESIAN_POINT('',(11.,-1.2,6.52132034));
#5343=CARTESIAN_POINT('',(11.,-1.2,5.52132034));
#5344=CARTESIAN_POINT('Origin',(11.,1.2,5.52132034));
#5345=CARTESIAN_POINT('',(9.,1.2,6.52132034));
#5346=CARTESIAN_POINT('',(9.,1.2,5.52132034));
#5347=CARTESIAN_POINT('',(11.,1.2,6.52132034));
#5348=CARTESIAN_POINT('Origin',(9.,-1.2,5.52132034));
#5349=CARTESIAN_POINT('',(9.,-1.2,6.52132034));
#5350=CARTESIAN_POINT('',(9.,-1.2,6.52132034));
#5351=CARTESIAN_POINT('',(9.,-1.2,5.52132034));
#5352=CARTESIAN_POINT('Origin',(9.,1.2,5.52132034));
#5353=CARTESIAN_POINT('',(9.,1.2,6.52132034));
#5354=CARTESIAN_POINT('Origin',(10.,0.,6.52132034));
#5355=CARTESIAN_POINT('',(0.,0.,0.));
#5356=CARTESIAN_POINT('Origin',(3.,0.,4.62132034355964));
#5357=CARTESIAN_POINT('',(17.,-1.83697019872103E-16,6.12132034355964));
#5358=CARTESIAN_POINT('Origin',(17.,0.,4.62132034355964));
#5359=CARTESIAN_POINT('',(3.,-1.83697019872103E-16,6.12132034355964));
#5360=CARTESIAN_POINT('',(3.,-1.83697019872103E-16,6.12132034355964));
#5361=CARTESIAN_POINT('Origin',(3.,0.,4.62132034355964));
#5362=CARTESIAN_POINT('Origin',(17.,0.,4.62132034355964));
#5363=CARTESIAN_POINT('Origin',(3.,0.,4.62132034355964));
#5364=CARTESIAN_POINT('',(0.,0.,0.));
#5365=CARTESIAN_POINT('Origin',(0.0866025403784439,-0.4,-0.15));
#5366=CARTESIAN_POINT('',(0.173205080756888,-0.4,0.));
#5367=CARTESIAN_POINT('',(0.0866025403784439,-0.4,-0.15));
#5368=CARTESIAN_POINT('',(0.173205080756888,-0.4,0.));
#5369=CARTESIAN_POINT('',(0.0866025403784439,-0.64,-0.15));
#5370=CARTESIAN_POINT('',(0.0866025403784439,-0.4,-0.15));
#5371=CARTESIAN_POINT('',(0.173205080756888,-0.64,0.));
#5372=CARTESIAN_POINT('',(0.173205080756888,-0.64,0.));
#5373=CARTESIAN_POINT('',(0.173205080756888,-0.4,0.));
#5374=CARTESIAN_POINT('Origin',(-0.0866025403784438,-0.4,-0.15));
#5375=CARTESIAN_POINT('',(-0.0866025403784438,-0.4,-0.15));
#5376=CARTESIAN_POINT('',(0.0866025403784439,-0.4,-0.15));
#5377=CARTESIAN_POINT('',(-0.0866025403784438,-0.64,-0.15));
#5378=CARTESIAN_POINT('',(-0.0866025403784438,-0.4,-0.15));
#5379=CARTESIAN_POINT('',(0.0866025403784439,-0.64,-0.15));
#5380=CARTESIAN_POINT('Origin',(-0.173205080756888,-0.4,-2.77555756156289E-17));
#5381=CARTESIAN_POINT('',(-0.173205080756888,-0.4,-2.12115047744981E-17));
#5382=CARTESIAN_POINT('',(-0.0866025403784438,-0.4,-0.15));
#5383=CARTESIAN_POINT('',(-0.173205080756888,-0.64,-2.77555756156289E-17));
#5384=CARTESIAN_POINT('',(-0.173205080756888,-0.4,-2.12115047744981E-17));
#5385=CARTESIAN_POINT('',(-0.0866025403784438,-0.64,-0.15));
#5386=CARTESIAN_POINT('Origin',(-0.0866025403784439,-0.4,0.15));
#5387=CARTESIAN_POINT('',(-0.0866025403784439,-0.4,0.15));
#5388=CARTESIAN_POINT('',(-0.173205080756888,-0.4,-2.12115047744981E-17));
#5389=CARTESIAN_POINT('',(-0.0866025403784439,-0.64,0.15));
#5390=CARTESIAN_POINT('',(-0.0866025403784439,-0.4,0.15));
#5391=CARTESIAN_POINT('',(-0.173205080756888,-0.64,-2.12115047744981E-17));
#5392=CARTESIAN_POINT('Origin',(0.0866025403784439,-0.4,0.15));
#5393=CARTESIAN_POINT('',(0.0866025403784439,-0.4,0.15));
#5394=CARTESIAN_POINT('',(-0.0866025403784439,-0.4,0.15));
#5395=CARTESIAN_POINT('',(0.0866025403784439,-0.64,0.15));
#5396=CARTESIAN_POINT('',(0.0866025403784439,-0.4,0.15));
#5397=CARTESIAN_POINT('',(-0.0866025403784439,-0.64,0.15));
#5398=CARTESIAN_POINT('Origin',(0.173205080756888,-0.4,0.));
#5399=CARTESIAN_POINT('',(0.0866025403784439,-0.4,0.15));
#5400=CARTESIAN_POINT('',(0.0866025403784439,-0.64,0.15));
#5401=CARTESIAN_POINT('Origin',(0.,-0.4,-2.77555756156289E-17));
#5402=CARTESIAN_POINT('Origin',(0.,-0.64,-2.77555756156289E-17));
#5403=CARTESIAN_POINT('Origin',(0.,-1.,0.));
#5404=CARTESIAN_POINT('',(-0.1954,-1.,2.39295984553393E-17));
#5405=CARTESIAN_POINT('Origin',(0.,-1.,0.));
#5406=CARTESIAN_POINT('Origin',(0.3,0.4,0.));
#5407=CARTESIAN_POINT('',(-0.3,0.4,-3.67394039744206E-17));
#5408=CARTESIAN_POINT('Origin',(0.,0.4,0.));
#5409=CARTESIAN_POINT('Origin',(0.,0.375,0.));
#5410=CARTESIAN_POINT('',(-0.35,0.35,-4.28626379701573E-17));
#5411=CARTESIAN_POINT('Origin',(0.,0.35,0.));
#5412=CARTESIAN_POINT('',(-0.325,0.375,-3.9801020972289E-17));
#5413=CARTESIAN_POINT('Origin',(0.,0.19,0.));
#5414=CARTESIAN_POINT('',(-0.35,0.03,-4.28626379701574E-17));
#5415=CARTESIAN_POINT('Origin',(0.,0.03,0.));
#5416=CARTESIAN_POINT('',(-0.35,0.19,-4.28626379701574E-17));
#5417=CARTESIAN_POINT('Origin',(0.,0.0149999999999999,0.));
#5418=CARTESIAN_POINT('',(-0.32,-3.29597460435593E-17,-3.91886975727153E-17));
#5419=CARTESIAN_POINT('Origin',(0.,0.,0.));
#5420=CARTESIAN_POINT('',(-0.335,0.0149999999999999,-4.10256677714363E-17));
#5421=CARTESIAN_POINT('Origin',(0.22,0.,0.));
#5422=CARTESIAN_POINT('',(-0.22,-6.93889390390723E-18,-2.69422295812418E-17));
#5423=CARTESIAN_POINT('Origin',(0.,0.,0.));
#5424=CARTESIAN_POINT('Origin',(0.,-0.02,0.));
#5425=CARTESIAN_POINT('',(-0.1954,-0.0492,2.39295984553393E-17));
#5426=CARTESIAN_POINT('Origin',(0.,-0.0492,0.));
#5427=CARTESIAN_POINT('',(-0.21,-0.02,-2.57175827820944E-17));
#5428=CARTESIAN_POINT('Origin',(0.,-0.8,0.));
#5429=CARTESIAN_POINT('',(-0.1954,-0.8,-2.39295984553393E-17));
#5430=CARTESIAN_POINT('',(0.,0.,0.));
#5431=CARTESIAN_POINT('Origin',(10.,-4.,0.));
#5432=CARTESIAN_POINT('',(9.6067,-4.,8.3));
#5433=CARTESIAN_POINT('Origin',(10.,-4.,8.3));
#5434=CARTESIAN_POINT('',(9.6067,-4.,0.));
#5435=CARTESIAN_POINT('',(9.6067,-4.,0.));
#5436=CARTESIAN_POINT('Origin',(10.,-4.,0.));
#5437=CARTESIAN_POINT('Origin',(10.,-4.,8.3));
#5438=CARTESIAN_POINT('Origin',(10.,-4.,0.));
#5439=CARTESIAN_POINT('',(0.,0.,0.));
#5440=CARTESIAN_POINT('Origin',(0.,0.,0.));
#5441=CARTESIAN_POINT('',(-0.42,0.16,5.14351655641888E-17));
#5442=CARTESIAN_POINT('Origin',(0.,0.16,0.));
#5443=CARTESIAN_POINT('',(-0.42,0.,5.14351655641888E-17));
#5444=CARTESIAN_POINT('',(-0.42,0.,5.14351655641888E-17));
#5445=CARTESIAN_POINT('Origin',(0.,0.,0.));
#5446=CARTESIAN_POINT('Origin',(0.,0.,0.));
#5447=CARTESIAN_POINT('',(-0.8,0.16,9.79717439317883E-17));
#5448=CARTESIAN_POINT('Origin',(0.,0.16,0.));
#5449=CARTESIAN_POINT('',(-0.8,0.,9.79717439317883E-17));
#5450=CARTESIAN_POINT('',(-0.8,0.,9.79717439317883E-17));
#5451=CARTESIAN_POINT('Origin',(0.,0.,0.));
#5452=CARTESIAN_POINT('Origin',(0.,0.16,0.));
#5453=CARTESIAN_POINT('Origin',(0.,0.,0.));
#5454=CARTESIAN_POINT('',(0.,0.,0.));
#5455=CARTESIAN_POINT('Origin',(0.,0.067277284513851,0.));
#5456=CARTESIAN_POINT('',(-0.375277674973257,0.0768195421087395,0.65));
#5457=CARTESIAN_POINT('',(0.375277674973257,0.0768195421087395,0.65));
#5458=CARTESIAN_POINT('Ctrl Pts',(-0.375277674973257,0.0768195421087395,
0.65));
#5459=CARTESIAN_POINT('Ctrl Pts',(1.66533453693773E-13,-0.0315137912242439,
0.65));
#5460=CARTESIAN_POINT('Ctrl Pts',(0.375277674973257,0.0768195421087394,
0.65));
#5461=CARTESIAN_POINT('',(-0.750555349946514,0.0768195421087394,-9.19165206894919E-17));
#5462=CARTESIAN_POINT('Ctrl Pts',(-0.750555349946514,0.0768195421087394,
-9.19165206894919E-17));
#5463=CARTESIAN_POINT('Ctrl Pts',(-0.562916512459802,-0.0315137912242434,
0.325000000000144));
#5464=CARTESIAN_POINT('Ctrl Pts',(-0.375277674973257,0.0768195421087395,
0.65));
#5465=CARTESIAN_POINT('',(-0.6175,-2.77555756156289E-17,-7.5621939847349E-17));
#5466=CARTESIAN_POINT('',(-0.734027674973257,0.067277284513851,-8.98924642641573E-17));
#5467=CARTESIAN_POINT('Origin',(0.,0.,0.));
#5468=CARTESIAN_POINT('',(-0.375277674973257,0.0768195421087395,-0.65));
#5469=CARTESIAN_POINT('Ctrl Pts',(-0.375277674973257,0.0768195421087395,
-0.65));
#5470=CARTESIAN_POINT('Ctrl Pts',(-0.562916512459968,-0.0315137912242437,
-0.324999999999856));
#5471=CARTESIAN_POINT('Ctrl Pts',(-0.750555349946514,0.0768195421087395,
-9.19165206894919E-17));
#5472=CARTESIAN_POINT('',(0.375277674973257,0.0768195421087395,-0.65));
#5473=CARTESIAN_POINT('Ctrl Pts',(0.375277674973257,0.0768195421087395,
-0.65));
#5474=CARTESIAN_POINT('Ctrl Pts',(-1.66144875635155E-13,-0.0315137912242437,
-0.65));
#5475=CARTESIAN_POINT('Ctrl Pts',(-0.375277674973257,0.0768195421087395,
-0.65));
#5476=CARTESIAN_POINT('',(0.750555349946514,0.0768195421087394,0.));
#5477=CARTESIAN_POINT('Ctrl Pts',(0.750555349946514,0.0768195421087394,
0.));
#5478=CARTESIAN_POINT('Ctrl Pts',(0.562916512459802,-0.0315137912242436,
-0.325000000000144));
#5479=CARTESIAN_POINT('Ctrl Pts',(0.375277674973257,0.0768195421087395,
-0.65));
#5480=CARTESIAN_POINT('Ctrl Pts',(0.375277674973257,0.0768195421087394,
0.65));
#5481=CARTESIAN_POINT('Ctrl Pts',(0.562916512459968,-0.0315137912242439,
0.324999999999856));
#5482=CARTESIAN_POINT('Ctrl Pts',(0.750555349946514,0.0768195421087394,
0.));
#5483=CARTESIAN_POINT('Origin',(0.,0.612722715486149,0.));
#5484=CARTESIAN_POINT('',(-0.6175,0.68,-7.5621939847349E-17));
#5485=CARTESIAN_POINT('Origin',(0.,0.68,0.));
#5486=CARTESIAN_POINT('',(-0.750555349946514,0.603180457891261,-9.19165206894919E-17));
#5487=CARTESIAN_POINT('',(-0.734027674973257,0.612722715486149,-8.98924642641573E-17));
#5488=CARTESIAN_POINT('',(-0.375277674973257,0.603180457891261,0.65));
#5489=CARTESIAN_POINT('Ctrl Pts',(-0.375277674973257,0.603180457891261,
0.65));
#5490=CARTESIAN_POINT('Ctrl Pts',(-0.562916512459968,0.711513791224243,
0.324999999999856));
#5491=CARTESIAN_POINT('Ctrl Pts',(-0.750555349946514,0.603180457891261,
-9.19165206894919E-17));
#5492=CARTESIAN_POINT('',(0.375277674973257,0.603180457891261,0.65));
#5493=CARTESIAN_POINT('Ctrl Pts',(0.375277674973257,0.603180457891261,0.65));
#5494=CARTESIAN_POINT('Ctrl Pts',(-1.66755498298699E-13,0.711513791224244,
0.65));
#5495=CARTESIAN_POINT('Ctrl Pts',(-0.375277674973257,0.603180457891261,
0.65));
#5496=CARTESIAN_POINT('',(0.750555349946514,0.603180457891261,0.));
#5497=CARTESIAN_POINT('Ctrl Pts',(0.750555349946514,0.603180457891261,0.));
#5498=CARTESIAN_POINT('Ctrl Pts',(0.562916512459802,0.711513791224244,0.325000000000144));
#5499=CARTESIAN_POINT('Ctrl Pts',(0.375277674973257,0.603180457891261,0.65));
#5500=CARTESIAN_POINT('',(0.375277674973257,0.603180457891261,-0.65));
#5501=CARTESIAN_POINT('Ctrl Pts',(0.375277674973257,0.603180457891261,-0.65));
#5502=CARTESIAN_POINT('Ctrl Pts',(0.562916512459969,0.711513791224244,-0.324999999999856));
#5503=CARTESIAN_POINT('Ctrl Pts',(0.750555349946514,0.603180457891261,0.));
#5504=CARTESIAN_POINT('',(-0.375277674973257,0.603180457891261,-0.65));
#5505=CARTESIAN_POINT('Ctrl Pts',(-0.375277674973257,0.603180457891261,
-0.65));
#5506=CARTESIAN_POINT('Ctrl Pts',(1.66422431391311E-13,0.711513791224244,
-0.65));
#5507=CARTESIAN_POINT('Ctrl Pts',(0.375277674973257,0.603180457891261,-0.65));
#5508=CARTESIAN_POINT('Ctrl Pts',(-0.750555349946514,0.603180457891261,
-9.19165206894919E-17));
#5509=CARTESIAN_POINT('Ctrl Pts',(-0.562916512459802,0.711513791224244,
-0.325000000000144));
#5510=CARTESIAN_POINT('Ctrl Pts',(-0.375277674973257,0.603180457891261,
-0.65));
#5511=CARTESIAN_POINT('Origin',(0.375277674973257,0.,-0.65));
#5512=CARTESIAN_POINT('',(-0.375277674973257,0.,-0.65));
#5513=CARTESIAN_POINT('',(0.375277674973257,0.,-0.65));
#5514=CARTESIAN_POINT('Origin',(-0.375277674973257,0.,-0.65));
#5515=CARTESIAN_POINT('',(-0.750555349946514,0.,-9.19165206894919E-17));
#5516=CARTESIAN_POINT('Origin',(-0.750555349946514,0.,-9.19165206894919E-17));
#5517=CARTESIAN_POINT('',(-0.375277674973257,0.,0.65));
#5518=CARTESIAN_POINT('Origin',(0.,0.,0.));
#5519=CARTESIAN_POINT('',(-0.338975,0.68,4.15124648740974E-17));
#5520=CARTESIAN_POINT('Origin',(0.,0.68,0.));
#5521=CARTESIAN_POINT('',(-0.338975,0.,4.15124648740974E-17));
#5522=CARTESIAN_POINT('',(-0.338975,0.,4.15124648740974E-17));
#5523=CARTESIAN_POINT('Origin',(0.,0.,0.));
#5524=CARTESIAN_POINT('Origin',(-0.375277674973257,0.,0.65));
#5525=CARTESIAN_POINT('',(0.375277674973257,0.,0.65));
#5526=CARTESIAN_POINT('Origin',(0.750555349946514,0.,0.));
#5527=CARTESIAN_POINT('',(0.750555349946514,0.,0.));
#5528=CARTESIAN_POINT('Origin',(0.375277674973257,0.,0.65));
#5529=CARTESIAN_POINT('Origin',(0.,0.68,-1.11022302462516E-16));
#5530=CARTESIAN_POINT('Origin',(0.,0.,-1.11022302462516E-16));
#5531=CARTESIAN_POINT('',(0.,0.,0.));
#5532=CARTESIAN_POINT('Origin',(6.5,-5.73205080756888,7.22132034));
#5533=CARTESIAN_POINT('',(6.89841665441537,-5.69649564641799,8.48132034));
#5534=CARTESIAN_POINT('',(6.89841665441537,-5.69649564641799,7.28132034));
#5535=CARTESIAN_POINT('',(6.89841665441537,-5.69649564641799,7.22132034));
#5536=CARTESIAN_POINT('',(6.33158334558463,-5.36923428297892,8.48132034));
#5537=CARTESIAN_POINT('Origin',(6.5,-5.73205080756888,8.48132034));
#5538=CARTESIAN_POINT('',(6.33158334558463,-5.36923428297892,7.28132034));
#5539=CARTESIAN_POINT('',(6.33158334558463,-5.36923428297892,7.22132034));
#5540=CARTESIAN_POINT('Origin',(6.5,-5.73205080756888,7.28132034));
#5541=CARTESIAN_POINT('Origin',(9.5,-4.,7.22132034));
#5542=CARTESIAN_POINT('',(9.27,-4.32726136343907,7.28132034));
#5543=CARTESIAN_POINT('',(9.27,-4.32726136343907,8.48132034));
#5544=CARTESIAN_POINT('',(9.27,-4.32726136343907,7.22132034));
#5545=CARTESIAN_POINT('',(9.27,-3.67273863656093,7.28132034));
#5546=CARTESIAN_POINT('Origin',(9.5,-4.,7.28132034));
#5547=CARTESIAN_POINT('',(9.27,-3.67273863656093,8.48132034));
#5548=CARTESIAN_POINT('',(9.27,-3.67273863656093,7.22132034));
#5549=CARTESIAN_POINT('Origin',(9.5,-4.,8.48132034));
#5550=CARTESIAN_POINT('Origin',(8.5,-2.26794919243112,7.22132034));
#5551=CARTESIAN_POINT('',(8.10158334558463,-2.30350435358201,8.48132034));
#5552=CARTESIAN_POINT('',(8.10158334558463,-2.30350435358201,7.28132034));
#5553=CARTESIAN_POINT('',(8.10158334558463,-2.30350435358201,7.22132034));
#5554=CARTESIAN_POINT('',(8.66841665441537,-2.63076571702108,8.48132034));
#5555=CARTESIAN_POINT('Origin',(8.5,-2.26794919243112,8.48132034));
#5556=CARTESIAN_POINT('',(8.66841665441537,-2.63076571702108,7.28132034));
#5557=CARTESIAN_POINT('',(8.66841665441537,-2.63076571702108,7.22132034));
#5558=CARTESIAN_POINT('Origin',(8.5,-2.26794919243112,7.28132034));
#5559=CARTESIAN_POINT('Origin',(6.5,-2.26794919243112,7.22132034));
#5560=CARTESIAN_POINT('',(6.33158334558463,-2.63076571702108,8.48132034));
#5561=CARTESIAN_POINT('',(6.33158334558463,-2.63076571702108,7.28132034));
#5562=CARTESIAN_POINT('',(6.33158334558463,-2.63076571702108,7.22132034));
#5563=CARTESIAN_POINT('',(6.89841665441537,-2.30350435358201,8.48132034));
#5564=CARTESIAN_POINT('Origin',(6.5,-2.26794919243112,8.48132034));
#5565=CARTESIAN_POINT('',(6.89841665441537,-2.30350435358201,7.28132034));
#5566=CARTESIAN_POINT('',(6.89841665441537,-2.30350435358201,7.22132034));
#5567=CARTESIAN_POINT('Origin',(6.5,-2.26794919243112,7.28132034));
#5568=CARTESIAN_POINT('Origin',(5.5,-4.,7.22132034));
#5569=CARTESIAN_POINT('',(5.73,-4.32726136343907,8.48132034));
#5570=CARTESIAN_POINT('',(5.73,-4.32726136343907,7.28132034));
#5571=CARTESIAN_POINT('',(5.73,-4.32726136343907,7.22132034));
#5572=CARTESIAN_POINT('',(5.73,-3.67273863656093,8.48132034));
#5573=CARTESIAN_POINT('Origin',(5.5,-4.,8.48132034));
#5574=CARTESIAN_POINT('',(5.73,-3.67273863656093,7.28132034));
#5575=CARTESIAN_POINT('',(5.73,-3.67273863656093,7.22132034));
#5576=CARTESIAN_POINT('Origin',(5.5,-4.,7.28132034));
#5577=CARTESIAN_POINT('Origin',(8.5,-5.73205080756888,7.22132034));
#5578=CARTESIAN_POINT('',(8.66841665441537,-5.36923428297892,8.48132034));
#5579=CARTESIAN_POINT('',(8.66841665441537,-5.36923428297892,7.28132034));
#5580=CARTESIAN_POINT('',(8.66841665441537,-5.36923428297892,7.22132034));
#5581=CARTESIAN_POINT('',(8.10158334558463,-5.69649564641799,8.48132034));
#5582=CARTESIAN_POINT('Origin',(8.5,-5.73205080756888,8.48132034));
#5583=CARTESIAN_POINT('',(8.10158334558463,-5.69649564641799,7.28132034));
#5584=CARTESIAN_POINT('',(8.10158334558463,-5.69649564641799,7.22132034));
#5585=CARTESIAN_POINT('Origin',(8.5,-5.73205080756888,7.28132034));
#5586=CARTESIAN_POINT('Origin',(7.5,-4.,8.48132034));
#5587=CARTESIAN_POINT('Origin',(7.5,-4.,8.48132034));
#5588=CARTESIAN_POINT('Origin',(7.5,-4.,8.48132034));
#5589=CARTESIAN_POINT('Origin',(7.5,-4.,8.48132034));
#5590=CARTESIAN_POINT('Origin',(7.5,-4.,8.48132034));
#5591=CARTESIAN_POINT('Origin',(7.5,-4.,8.48132034));
#5592=CARTESIAN_POINT('Origin',(7.5,-4.,8.48132034));
#5593=CARTESIAN_POINT('',(7.075,-4.,8.48132034));
#5594=CARTESIAN_POINT('Origin',(7.5,-4.,8.48132034));
#5595=CARTESIAN_POINT('Origin',(7.5,-4.,7.28132034));
#5596=CARTESIAN_POINT('Origin',(7.5,-4.,7.28132034));
#5597=CARTESIAN_POINT('Origin',(7.5,-4.,7.28132034));
#5598=CARTESIAN_POINT('Origin',(7.5,-4.,7.28132034));
#5599=CARTESIAN_POINT('Origin',(7.5,-4.,7.28132034));
#5600=CARTESIAN_POINT('Origin',(7.5,-4.,7.28132034));
#5601=CARTESIAN_POINT('Origin',(7.5,-4.,7.28132034));
#5602=CARTESIAN_POINT('Origin',(7.5,-4.,7.28132034));
#5603=CARTESIAN_POINT('Origin',(7.5,-4.,7.28132034));
#5604=CARTESIAN_POINT('Origin',(7.5,-4.,7.28132034));
#5605=CARTESIAN_POINT('Origin',(7.5,-4.,7.28132034));
#5606=CARTESIAN_POINT('Origin',(7.5,-4.,7.28132034));
#5607=CARTESIAN_POINT('Origin',(7.87527767497326,-3.35,7.27132034));
#5608=CARTESIAN_POINT('',(7.87527767497326,-3.35,7.28132034));
#5609=CARTESIAN_POINT('',(7.12472232502674,-3.35,7.28132034));
#5610=CARTESIAN_POINT('',(7.68763883748663,-3.35,7.28132034));
#5611=CARTESIAN_POINT('',(7.87527767497326,-3.35,7.97132034));
#5612=CARTESIAN_POINT('',(7.87527767497326,-3.35,7.27132034));
#5613=CARTESIAN_POINT('',(7.12472232502674,-3.35,7.97132034));
#5614=CARTESIAN_POINT('',(7.87527767497326,-3.35,7.97132034));
#5615=CARTESIAN_POINT('',(7.12472232502674,-3.35,7.27132034));
#5616=CARTESIAN_POINT('Origin',(7.12472232502674,-3.35,7.27132034));
#5617=CARTESIAN_POINT('',(6.74944465005349,-4.,7.28132034));
#5618=CARTESIAN_POINT('',(7.03090290628343,-3.5125,7.28132034));
#5619=CARTESIAN_POINT('',(6.74944465005349,-4.,7.97132034));
#5620=CARTESIAN_POINT('',(7.12472232502674,-3.35,7.97132034));
#5621=CARTESIAN_POINT('',(6.74944465005349,-4.,7.27132034));
#5622=CARTESIAN_POINT('Origin',(6.74944465005349,-4.,7.27132034));
#5623=CARTESIAN_POINT('',(7.12472232502674,-4.65,7.28132034));
#5624=CARTESIAN_POINT('',(6.8432640687968,-4.1625,7.28132034));
#5625=CARTESIAN_POINT('',(7.12472232502674,-4.65,7.97132034));
#5626=CARTESIAN_POINT('',(6.74944465005349,-4.,7.97132034));
#5627=CARTESIAN_POINT('',(7.12472232502674,-4.65,7.27132034));
#5628=CARTESIAN_POINT('Origin',(7.12472232502674,-4.65,7.27132034));
#5629=CARTESIAN_POINT('',(7.87527767497326,-4.65,7.28132034));
#5630=CARTESIAN_POINT('',(7.31236116251337,-4.65,7.28132034));
#5631=CARTESIAN_POINT('',(7.87527767497326,-4.65,7.97132034));
#5632=CARTESIAN_POINT('',(7.12472232502674,-4.65,7.97132034));
#5633=CARTESIAN_POINT('',(7.87527767497326,-4.65,7.27132034));
#5634=CARTESIAN_POINT('Origin',(8.25055534994651,-4.,7.27132034));
#5635=CARTESIAN_POINT('',(8.25055534994651,-4.,7.28132034));
#5636=CARTESIAN_POINT('',(8.1567359312032,-3.8375,7.28132034));
#5637=CARTESIAN_POINT('',(8.25055534994651,-4.,7.97132034));
#5638=CARTESIAN_POINT('',(8.25055534994651,-4.,7.27132034));
#5639=CARTESIAN_POINT('',(8.25055534994651,-4.,7.97132034));
#5640=CARTESIAN_POINT('Origin',(7.87527767497326,-4.65,7.27132034));
#5641=CARTESIAN_POINT('',(7.96909709371657,-4.4875,7.28132034));
#5642=CARTESIAN_POINT('',(7.87527767497326,-4.65,7.97132034));
#5643=CARTESIAN_POINT('Origin',(7.5,-4.,7.97132034));
#5644=CARTESIAN_POINT('',(7.075,-4.,7.97132034));
#5645=CARTESIAN_POINT('Origin',(7.5,-4.,7.97132034));
#5646=CARTESIAN_POINT('Origin',(7.5,-4.,7.28132034));
#5647=CARTESIAN_POINT('',(7.075,-4.,7.28132034));
#5648=CARTESIAN_POINT('Origin',(7.5,-4.,7.28132034));
#5649=CARTESIAN_POINT('',(0.,0.,0.));
#5650=CARTESIAN_POINT('',(0.,0.,0.));
#5651=CARTESIAN_POINT('',(4.5,0.,0.7));
#5652=CARTESIAN_POINT('',(-2.,0.,0.));
#5653=CARTESIAN_POINT('',(4.5,-2.5,2.5));
#5654=CARTESIAN_POINT('',(4.5,2.5,2.5));
#5655=CARTESIAN_POINT('',(10.5,0.,0.7));
#5656=CARTESIAN_POINT('',(4.,0.,0.));
#5657=CARTESIAN_POINT('',(10.5,-2.5,2.5));
#5658=CARTESIAN_POINT('',(10.5,2.5,2.5));
#5659=CARTESIAN_POINT('',(-2.5,0.,0.));
#5660=CARTESIAN_POINT('',(-2.5,0.,0.));
#5661=CARTESIAN_POINT('',(-2.5,0.,0.));
#5662=CARTESIAN_POINT('',(7.5,-0.8,7.12132034355964));
#5663=CARTESIAN_POINT('',(7.5,0.8,7.12132034355964));
#5664=CARTESIAN_POINT('',(-2.5,0.,0.));
#5665=CARTESIAN_POINT('',(7.5,-4.,1.));
#5666=CARTESIAN_POINT('',(7.5,-4.,7.12132034355964));
#5667=CARTESIAN_POINT('',(7.5,-4.,1.16));
#5668=CARTESIAN_POINT('',(7.5,-4.,7.28132034355964));
#5669=CARTESIAN_POINT('',(-2.5,8.,0.));
#5670=CARTESIAN_POINT('',(7.5,4.,1.));
#5671=CARTESIAN_POINT('',(7.5,4.,7.12132034355964));
#5672=CARTESIAN_POINT('',(7.5,4.,1.16));
#5673=CARTESIAN_POINT('',(7.5,4.,7.28132034355964));
#5674=CARTESIAN_POINT('',(0.671714202456419,9.06206608679347,-0.159999999999998));
#5675=UNCERTAINTY_MEASURE_WITH_UNIT(LENGTH_MEASURE(0.001),#5703,
'DISTANCE_ACCURACY_VALUE',
'Maximum model space distance between geometric entities at asserted c
onnectivities');
#5676=UNCERTAINTY_MEASURE_WITH_UNIT(LENGTH_MEASURE(0.001),#5703,
'DISTANCE_ACCURACY_VALUE',
'Maximum model space distance between geometric entities at asserted c
onnectivities');
#5677=UNCERTAINTY_MEASURE_WITH_UNIT(LENGTH_MEASURE(0.001),#5703,
'DISTANCE_ACCURACY_VALUE',
'Maximum model space distance between geometric entities at asserted c
onnectivities');
#5678=UNCERTAINTY_MEASURE_WITH_UNIT(LENGTH_MEASURE(0.001),#5703,
'DISTANCE_ACCURACY_VALUE',
'Maximum model space distance between geometric entities at asserted c
onnectivities');
#5679=UNCERTAINTY_MEASURE_WITH_UNIT(LENGTH_MEASURE(0.001),#5703,
'DISTANCE_ACCURACY_VALUE',
'Maximum model space distance between geometric entities at asserted c
onnectivities');
#5680=UNCERTAINTY_MEASURE_WITH_UNIT(LENGTH_MEASURE(0.001),#5703,
'DISTANCE_ACCURACY_VALUE',
'Maximum model space distance between geometric entities at asserted c
onnectivities');
#5681=UNCERTAINTY_MEASURE_WITH_UNIT(LENGTH_MEASURE(0.001),#5703,
'DISTANCE_ACCURACY_VALUE',
'Maximum model space distance between geometric entities at asserted c
onnectivities');
#5682=UNCERTAINTY_MEASURE_WITH_UNIT(LENGTH_MEASURE(0.001),#5703,
'DISTANCE_ACCURACY_VALUE',
'Maximum model space distance between geometric entities at asserted c
onnectivities');
#5683=UNCERTAINTY_MEASURE_WITH_UNIT(LENGTH_MEASURE(0.001),#5703,
'DISTANCE_ACCURACY_VALUE',
'Maximum model space distance between geometric entities at asserted c
onnectivities');
#5684=UNCERTAINTY_MEASURE_WITH_UNIT(LENGTH_MEASURE(0.001),#5703,
'DISTANCE_ACCURACY_VALUE',
'Maximum model space distance between geometric entities at asserted c
onnectivities');
#5685=UNCERTAINTY_MEASURE_WITH_UNIT(LENGTH_MEASURE(0.001),#5703,
'DISTANCE_ACCURACY_VALUE',
'Maximum model space distance between geometric entities at asserted c
onnectivities');
#5686=UNCERTAINTY_MEASURE_WITH_UNIT(LENGTH_MEASURE(0.001),#5703,
'DISTANCE_ACCURACY_VALUE',
'Maximum model space distance between geometric entities at asserted c
onnectivities');
#5687=UNCERTAINTY_MEASURE_WITH_UNIT(LENGTH_MEASURE(0.001),#5703,
'DISTANCE_ACCURACY_VALUE',
'Maximum model space distance between geometric entities at asserted c
onnectivities');
#5688=UNCERTAINTY_MEASURE_WITH_UNIT(LENGTH_MEASURE(0.001),#5703,
'DISTANCE_ACCURACY_VALUE',
'Maximum model space distance between geometric entities at asserted c
onnectivities');
#5689=(
GEOMETRIC_REPRESENTATION_CONTEXT(3)
GLOBAL_UNCERTAINTY_ASSIGNED_CONTEXT((#5675))
GLOBAL_UNIT_ASSIGNED_CONTEXT((#5703,#5705,#5706))
REPRESENTATION_CONTEXT('','3D')
);
#5690=(
GEOMETRIC_REPRESENTATION_CONTEXT(3)
GLOBAL_UNCERTAINTY_ASSIGNED_CONTEXT((#5676))
GLOBAL_UNIT_ASSIGNED_CONTEXT((#5703,#5705,#5706))
REPRESENTATION_CONTEXT('','3D')
);
#5691=(
GEOMETRIC_REPRESENTATION_CONTEXT(3)
GLOBAL_UNCERTAINTY_ASSIGNED_CONTEXT((#5677))
GLOBAL_UNIT_ASSIGNED_CONTEXT((#5703,#5705,#5706))
REPRESENTATION_CONTEXT('','3D')
);
#5692=(
GEOMETRIC_REPRESENTATION_CONTEXT(3)
GLOBAL_UNCERTAINTY_ASSIGNED_CONTEXT((#5678))
GLOBAL_UNIT_ASSIGNED_CONTEXT((#5703,#5705,#5706))
REPRESENTATION_CONTEXT('','3D')
);
#5693=(
GEOMETRIC_REPRESENTATION_CONTEXT(3)
GLOBAL_UNCERTAINTY_ASSIGNED_CONTEXT((#5679))
GLOBAL_UNIT_ASSIGNED_CONTEXT((#5703,#5705,#5706))
REPRESENTATION_CONTEXT('','3D')
);
#5694=(
GEOMETRIC_REPRESENTATION_CONTEXT(3)
GLOBAL_UNCERTAINTY_ASSIGNED_CONTEXT((#5680))
GLOBAL_UNIT_ASSIGNED_CONTEXT((#5703,#5705,#5706))
REPRESENTATION_CONTEXT('','3D')
);
#5695=(
GEOMETRIC_REPRESENTATION_CONTEXT(3)
GLOBAL_UNCERTAINTY_ASSIGNED_CONTEXT((#5681))
GLOBAL_UNIT_ASSIGNED_CONTEXT((#5703,#5705,#5706))
REPRESENTATION_CONTEXT('','3D')
);
#5696=(
GEOMETRIC_REPRESENTATION_CONTEXT(3)
GLOBAL_UNCERTAINTY_ASSIGNED_CONTEXT((#5682))
GLOBAL_UNIT_ASSIGNED_CONTEXT((#5703,#5705,#5706))
REPRESENTATION_CONTEXT('','3D')
);
#5697=(
GEOMETRIC_REPRESENTATION_CONTEXT(3)
GLOBAL_UNCERTAINTY_ASSIGNED_CONTEXT((#5683))
GLOBAL_UNIT_ASSIGNED_CONTEXT((#5703,#5705,#5706))
REPRESENTATION_CONTEXT('','3D')
);
#5698=(
GEOMETRIC_REPRESENTATION_CONTEXT(3)
GLOBAL_UNCERTAINTY_ASSIGNED_CONTEXT((#5684))
GLOBAL_UNIT_ASSIGNED_CONTEXT((#5703,#5705,#5706))
REPRESENTATION_CONTEXT('','3D')
);
#5699=(
GEOMETRIC_REPRESENTATION_CONTEXT(3)
GLOBAL_UNCERTAINTY_ASSIGNED_CONTEXT((#5685))
GLOBAL_UNIT_ASSIGNED_CONTEXT((#5703,#5705,#5706))
REPRESENTATION_CONTEXT('','3D')
);
#5700=(
GEOMETRIC_REPRESENTATION_CONTEXT(3)
GLOBAL_UNCERTAINTY_ASSIGNED_CONTEXT((#5686))
GLOBAL_UNIT_ASSIGNED_CONTEXT((#5703,#5705,#5706))
REPRESENTATION_CONTEXT('','3D')
);
#5701=(
GEOMETRIC_REPRESENTATION_CONTEXT(3)
GLOBAL_UNCERTAINTY_ASSIGNED_CONTEXT((#5687))
GLOBAL_UNIT_ASSIGNED_CONTEXT((#5703,#5705,#5706))
REPRESENTATION_CONTEXT('','3D')
);
#5702=(
GEOMETRIC_REPRESENTATION_CONTEXT(3)
GLOBAL_UNCERTAINTY_ASSIGNED_CONTEXT((#5688))
GLOBAL_UNIT_ASSIGNED_CONTEXT((#5703,#5705,#5706))
REPRESENTATION_CONTEXT('','3D')
);
#5703=(
LENGTH_UNIT()
NAMED_UNIT(*)
SI_UNIT(.CENTI.,.METRE.)
);
#5704=(
LENGTH_UNIT()
NAMED_UNIT(*)
SI_UNIT($,.METRE.)
);
#5705=(
NAMED_UNIT(*)
PLANE_ANGLE_UNIT()
SI_UNIT($,.RADIAN.)
);
#5706=(
NAMED_UNIT(*)
SI_UNIT($,.STERADIAN.)
SOLID_ANGLE_UNIT()
);
#5707=SHAPE_DEFINITION_REPRESENTATION(#5720,#5759);
#5708=SHAPE_DEFINITION_REPRESENTATION(#5721,#5760);
#5709=SHAPE_DEFINITION_REPRESENTATION(#5722,#5761);
#5710=SHAPE_DEFINITION_REPRESENTATION(#5723,#5762);
#5711=SHAPE_DEFINITION_REPRESENTATION(#5724,#5763);
#5712=SHAPE_DEFINITION_REPRESENTATION(#5725,#5764);
#5713=SHAPE_DEFINITION_REPRESENTATION(#5726,#5765);
#5714=SHAPE_DEFINITION_REPRESENTATION(#5727,#5766);
#5715=SHAPE_DEFINITION_REPRESENTATION(#5728,#5767);
#5716=SHAPE_DEFINITION_REPRESENTATION(#5729,#5768);
#5717=SHAPE_DEFINITION_REPRESENTATION(#5730,#5769);
#5718=SHAPE_DEFINITION_REPRESENTATION(#5731,#5770);
#5719=SHAPE_DEFINITION_REPRESENTATION(#5732,#5771);
#5720=PRODUCT_DEFINITION_SHAPE('',$,#5773);
#5721=PRODUCT_DEFINITION_SHAPE('',$,#5774);
#5722=PRODUCT_DEFINITION_SHAPE('',$,#5775);
#5723=PRODUCT_DEFINITION_SHAPE('',$,#5776);
#5724=PRODUCT_DEFINITION_SHAPE('',$,#5777);
#5725=PRODUCT_DEFINITION_SHAPE('',$,#5778);
#5726=PRODUCT_DEFINITION_SHAPE('',$,#5779);
#5727=PRODUCT_DEFINITION_SHAPE('',$,#5780);
#5728=PRODUCT_DEFINITION_SHAPE('',$,#5781);
#5729=PRODUCT_DEFINITION_SHAPE('',$,#5782);
#5730=PRODUCT_DEFINITION_SHAPE('',$,#5783);
#5731=PRODUCT_DEFINITION_SHAPE('',$,#5784);
#5732=PRODUCT_DEFINITION_SHAPE('',$,#5785);
#5733=PRODUCT_DEFINITION_SHAPE($,$,#89);
#5734=PRODUCT_DEFINITION_SHAPE($,$,#90);
#5735=PRODUCT_DEFINITION_SHAPE($,$,#91);
#5736=PRODUCT_DEFINITION_SHAPE($,$,#92);
#5737=PRODUCT_DEFINITION_SHAPE($,$,#93);
#5738=PRODUCT_DEFINITION_SHAPE($,$,#94);
#5739=PRODUCT_DEFINITION_SHAPE($,$,#95);
#5740=PRODUCT_DEFINITION_SHAPE($,$,#96);
#5741=PRODUCT_DEFINITION_SHAPE($,$,#97);
#5742=PRODUCT_DEFINITION_SHAPE($,$,#98);
#5743=PRODUCT_DEFINITION_SHAPE($,$,#99);
#5744=PRODUCT_DEFINITION_SHAPE($,$,#100);
#5745=PRODUCT_DEFINITION_SHAPE($,$,#101);
#5746=PRODUCT_DEFINITION_SHAPE($,$,#102);
#5747=PRODUCT_DEFINITION_SHAPE($,$,#103);
#5748=PRODUCT_DEFINITION_SHAPE($,$,#104);
#5749=PRODUCT_DEFINITION_SHAPE($,$,#105);
#5750=PRODUCT_DEFINITION_SHAPE($,$,#106);
#5751=PRODUCT_DEFINITION_SHAPE($,$,#107);
#5752=PRODUCT_DEFINITION_SHAPE($,$,#108);
#5753=PRODUCT_DEFINITION_SHAPE($,$,#109);
#5754=PRODUCT_DEFINITION_SHAPE($,$,#110);
#5755=PRODUCT_DEFINITION_SHAPE($,$,#111);
#5756=PRODUCT_DEFINITION_SHAPE($,$,#112);
#5757=PRODUCT_DEFINITION_SHAPE($,$,#113);
#5758=PRODUCT_DEFINITION_SHAPE($,$,#114);
#5759=SHAPE_REPRESENTATION('',(#3410,#3737,#3738,#3739,#3740,#3741,#3742,
#3743,#3744,#3745,#3746,#3747,#3748,#3749,#3750,#3751,#3752,#3753,#3754,
#3755,#3756,#3757,#3758,#3759,#3760,#3761,#3762),#5689);
#5760=SHAPE_REPRESENTATION('',(#3411),#5690);
#5761=SHAPE_REPRESENTATION('',(#3503),#5691);
#5762=SHAPE_REPRESENTATION('',(#3514),#5692);
#5763=SHAPE_REPRESENTATION('',(#3565),#5693);
#5764=SHAPE_REPRESENTATION('',(#3591),#5694);
#5765=SHAPE_REPRESENTATION('',(#3610),#5695);
#5766=SHAPE_REPRESENTATION('',(#3627),#5696);
#5767=SHAPE_REPRESENTATION('',(#3633),#5697);
#5768=SHAPE_REPRESENTATION('',(#3657),#5698);
#5769=SHAPE_REPRESENTATION('',(#3663),#5699);
#5770=SHAPE_REPRESENTATION('',(#3672),#5700);
#5771=SHAPE_REPRESENTATION('',(#3688),#5701);
#5772=PRODUCT_DEFINITION_CONTEXT('part definition',#5813,'design');
#5773=PRODUCT_DEFINITION('PAT-111',
'PAT-111',#5786,#5772);
#5774=PRODUCT_DEFINITION('Fixture grid plate','Fixture grid plate',
#5787,#5772);
#5775=PRODUCT_DEFINITION('Key 6x6x20','Key 6x6x20',#5788,#5772);
#5776=PRODUCT_DEFINITION('V block','V block',#5789,#5772);
#5777=PRODUCT_DEFINITION('Cap Screw - M6x25','Cap Screw - M6x25',
#5790,#5772);
#5778=PRODUCT_DEFINITION('Strap','Strap',#5791,#5772);
#5779=PRODUCT_DEFINITION('Replaceable contact pad',
'Replaceable contact pad',#5792,#5772);
#5780=PRODUCT_DEFINITION('Example round stock',
'Example round stock',#5793,#5772);
#5781=PRODUCT_DEFINITION('M4x10 Cap Screw','M4x10 Cap Screw',
#5794,#5772);
#5782=PRODUCT_DEFINITION('M8 clamp stud','M8 clamp stud',#5795,
#5772);
#5783=PRODUCT_DEFINITION('Flat Washer - M8','Flat Washer - M8',
#5796,#5772);
#5784=PRODUCT_DEFINITION('Hex Nut - M8','Hex Nut - M8',#5797,
#5772);
#5785=PRODUCT_DEFINITION('Captive-nut hand knob',
'Captive-nut hand knob',#5798,#5772);
#5786=PRODUCT_DEFINITION_FORMATION('',$,#5815);
#5787=PRODUCT_DEFINITION_FORMATION('',$,#5816);
#5788=PRODUCT_DEFINITION_FORMATION('',$,#5817);
#5789=PRODUCT_DEFINITION_FORMATION('',$,#5818);
#5790=PRODUCT_DEFINITION_FORMATION('',$,#5819);
#5791=PRODUCT_DEFINITION_FORMATION('',$,#5820);
#5792=PRODUCT_DEFINITION_FORMATION('',$,#5821);
#5793=PRODUCT_DEFINITION_FORMATION('',$,#5822);
#5794=PRODUCT_DEFINITION_FORMATION('',$,#5823);
#5795=PRODUCT_DEFINITION_FORMATION('',$,#5824);
#5796=PRODUCT_DEFINITION_FORMATION('',$,#5825);
#5797=PRODUCT_DEFINITION_FORMATION('',$,#5826);
#5798=PRODUCT_DEFINITION_FORMATION('',$,#5827);
#5799=PRODUCT_RELATED_PRODUCT_CATEGORY('PAT-111',
'PAT-111',(#5815));
#5800=PRODUCT_RELATED_PRODUCT_CATEGORY('Fixture grid plate',
'Fixture grid plate',(#5816));
#5801=PRODUCT_RELATED_PRODUCT_CATEGORY('Key 6x6x20','Key 6x6x20',(#5817));
#5802=PRODUCT_RELATED_PRODUCT_CATEGORY('V block','V block',(#5818));
#5803=PRODUCT_RELATED_PRODUCT_CATEGORY('Cap Screw - M6x25',
'Cap Screw - M6x25',(#5819));
#5804=PRODUCT_RELATED_PRODUCT_CATEGORY('Strap','Strap',(#5820));
#5805=PRODUCT_RELATED_PRODUCT_CATEGORY('Replaceable contact pad',
'Replaceable contact pad',(#5821));
#5806=PRODUCT_RELATED_PRODUCT_CATEGORY('Example round stock',
'Example round stock',(#5822));
#5807=PRODUCT_RELATED_PRODUCT_CATEGORY('M4x10 Cap Screw',
'M4x10 Cap Screw',(#5823));
#5808=PRODUCT_RELATED_PRODUCT_CATEGORY('M8 clamp stud','M8 clamp stud',
(#5824));
#5809=PRODUCT_RELATED_PRODUCT_CATEGORY('Flat Washer - M8',
'Flat Washer - M8',(#5825));
#5810=PRODUCT_RELATED_PRODUCT_CATEGORY('Hex Nut - M8','Hex Nut - M8',(#5826));
#5811=PRODUCT_RELATED_PRODUCT_CATEGORY('Captive-nut hand knob',
'Captive-nut hand knob',(#5827));
#5812=APPLICATION_PROTOCOL_DEFINITION('international standard',
'automotive_design',2009,#5813);
#5813=APPLICATION_CONTEXT(
'Core Data for Automotive Mechanical Design Process');
#5814=PRODUCT_CONTEXT('part definition',#5813,'mechanical');
#5815=PRODUCT('PAT-111','PAT-111',
'PAT-111',(#5814));
#5816=PRODUCT('Fixture grid plate','Fixture grid plate',
'Fixture grid plate',(#5814));
#5817=PRODUCT('Key 6x6x20','Key 6x6x20','Key 6x6x20',(#5814));
#5818=PRODUCT('V block','V block','V block',(#5814));
#5819=PRODUCT('Cap Screw - M6x25','Cap Screw - M6x25',
'Cap Screw - M6x25',(#5814));
#5820=PRODUCT('Strap','Strap','Strap',(#5814));
#5821=PRODUCT('Replaceable contact pad','Replaceable contact pad',
'Replaceable contact pad',(#5814));
#5822=PRODUCT('Example round stock','Example round stock',
'Example round stock',(#5814));
#5823=PRODUCT('M4x10 Cap Screw','M4x10 Cap Screw',
'M4x10 Cap Screw',(#5814));
#5824=PRODUCT('M8 clamp stud','M8 clamp stud',
'M8 clamp stud',(#5814));
#5825=PRODUCT('Flat Washer - M8','Flat Washer - M8',
'Flat Washer - M8',(#5814));
#5826=PRODUCT('Hex Nut - M8','Hex Nut - M8','Hex Nut - M8',
(#5814));
#5827=PRODUCT('Captive-nut hand knob','Captive-nut hand knob',
'Captive-nut hand knob',(#5814));
#5828=PRESENTATION_STYLE_ASSIGNMENT((#5834));
#5829=PRESENTATION_STYLE_ASSIGNMENT((#5835));
#5830=PRESENTATION_STYLE_ASSIGNMENT((#5836));
#5831=PRESENTATION_STYLE_ASSIGNMENT((#5837));
#5832=PRESENTATION_STYLE_ASSIGNMENT((#5838));
#5833=PRESENTATION_STYLE_ASSIGNMENT((#5839));
#5834=SURFACE_STYLE_USAGE(.BOTH.,#5840);
#5835=SURFACE_STYLE_USAGE(.BOTH.,#5841);
#5836=SURFACE_STYLE_USAGE(.BOTH.,#5842);
#5837=SURFACE_STYLE_USAGE(.BOTH.,#5843);
#5838=SURFACE_STYLE_USAGE(.BOTH.,#5844);
#5839=SURFACE_STYLE_USAGE(.BOTH.,#5845);
#5840=SURFACE_SIDE_STYLE('',(#5846));
#5841=SURFACE_SIDE_STYLE('',(#5847));
#5842=SURFACE_SIDE_STYLE('',(#5848));
#5843=SURFACE_SIDE_STYLE('',(#5849));
#5844=SURFACE_SIDE_STYLE('',(#5850));
#5845=SURFACE_SIDE_STYLE('',(#5851));
#5846=SURFACE_STYLE_FILL_AREA(#5852);
#5847=SURFACE_STYLE_FILL_AREA(#5853);
#5848=SURFACE_STYLE_FILL_AREA(#5854);
#5849=SURFACE_STYLE_FILL_AREA(#5855);
#5850=SURFACE_STYLE_FILL_AREA(#5856);
#5851=SURFACE_STYLE_FILL_AREA(#5857);
#5852=FILL_AREA_STYLE('Steel - Satin',(#5858));
#5853=FILL_AREA_STYLE('CAD Library Painted - Engineering blue',(#5859));
#5854=FILL_AREA_STYLE('CAD Library Painted - Steel gray',(#5860));
#5855=FILL_AREA_STYLE('CAD Library Painted - Light blue',(#5861));
#5856=FILL_AREA_STYLE('CAD Library Painted - Graphite',(#5862));
#5857=FILL_AREA_STYLE('CAD Library Painted - Off white',(#5863));
#5858=FILL_AREA_STYLE_COLOUR('Steel - Satin',#5864);
#5859=FILL_AREA_STYLE_COLOUR('CAD Library Painted - Engineering blue',#5865);
#5860=FILL_AREA_STYLE_COLOUR('CAD Library Painted - Steel gray',#5866);
#5861=FILL_AREA_STYLE_COLOUR('CAD Library Painted - Light blue',#5867);
#5862=FILL_AREA_STYLE_COLOUR('CAD Library Painted - Graphite',#5868);
#5863=FILL_AREA_STYLE_COLOUR('CAD Library Painted - Off white',#5869);
#5864=COLOUR_RGB('Steel - Satin',0.627450980392157,0.627450980392157,0.627450980392157);
#5865=COLOUR_RGB('CAD Library Painted - Engineering blue',0.12156862745098,
0.356862745098039,0.6);
#5866=COLOUR_RGB('CAD Library Painted - Steel gray',0.592156862745098,0.631372549019608,
0.67843137254902);
#5867=COLOUR_RGB('CAD Library Painted - Light blue',0.286274509803922,0.552941176470588,
0.780392156862745);
#5868=COLOUR_RGB('CAD Library Painted - Graphite',0.0980392156862745,0.109803921568627,
0.125490196078431);
#5869=COLOUR_RGB('CAD Library Painted - Off white',0.909803921568627,0.901960784313726,
0.858823529411765);
#5870=COLOUR_RGB('Dark Blue',0.08,0.2,0.34);
#5871=FILL_AREA_STYLE_COLOUR('',#5870);
#5872=FILL_AREA_STYLE('',(#5871));
#5873=SURFACE_STYLE_FILL_AREA(#5872);
#5874=SURFACE_SIDE_STYLE('',(#5873));
#5875=SURFACE_STYLE_USAGE(.BOTH.,#5874);
#5876=PRESENTATION_STYLE_ASSIGNMENT((#5875));
#5877=COLOUR_RGB('Light Blue',0.38,0.62,0.78);
#5878=FILL_AREA_STYLE_COLOUR('',#5877);
#5879=FILL_AREA_STYLE('',(#5878));
#5880=SURFACE_STYLE_FILL_AREA(#5879);
#5881=SURFACE_SIDE_STYLE('',(#5880));
#5882=SURFACE_STYLE_USAGE(.BOTH.,#5881);
#5883=PRESENTATION_STYLE_ASSIGNMENT((#5882));
#5884=COLOUR_RGB('Sky Blue',0.24,0.69,0.87);
#5885=FILL_AREA_STYLE_COLOUR('',#5884);
#5886=FILL_AREA_STYLE('',(#5885));
#5887=SURFACE_STYLE_FILL_AREA(#5886);
#5888=SURFACE_SIDE_STYLE('',(#5887));
#5889=SURFACE_STYLE_USAGE(.BOTH.,#5888);
#5890=PRESENTATION_STYLE_ASSIGNMENT((#5889));
#5891=COLOUR_RGB('Grey',0.48,0.52,0.57);
#5892=FILL_AREA_STYLE_COLOUR('',#5891);
#5893=FILL_AREA_STYLE('',(#5892));
#5894=SURFACE_STYLE_FILL_AREA(#5893);
#5895=SURFACE_SIDE_STYLE('',(#5894));
#5896=SURFACE_STYLE_USAGE(.BOTH.,#5895);
#5897=PRESENTATION_STYLE_ASSIGNMENT((#5896));
#5898=COLOUR_RGB('Black',0.12,0.14,0.17);
#5899=FILL_AREA_STYLE_COLOUR('',#5898);
#5900=FILL_AREA_STYLE('',(#5899));
#5901=SURFACE_STYLE_FILL_AREA(#5900);
#5902=SURFACE_SIDE_STYLE('',(#5901));
#5903=SURFACE_STYLE_USAGE(.BOTH.,#5902);
#5904=PRESENTATION_STYLE_ASSIGNMENT((#5903));
#5905=COLOUR_RGB('Off White',0.89,0.88,0.83);
#5906=FILL_AREA_STYLE_COLOUR('',#5905);
#5907=FILL_AREA_STYLE('',(#5906));
#5908=SURFACE_STYLE_FILL_AREA(#5907);
#5909=SURFACE_SIDE_STYLE('',(#5908));
#5910=SURFACE_STYLE_USAGE(.BOTH.,#5909);
#5911=PRESENTATION_STYLE_ASSIGNMENT((#5910));
ENDSEC;
END-ISO-10303-21;
